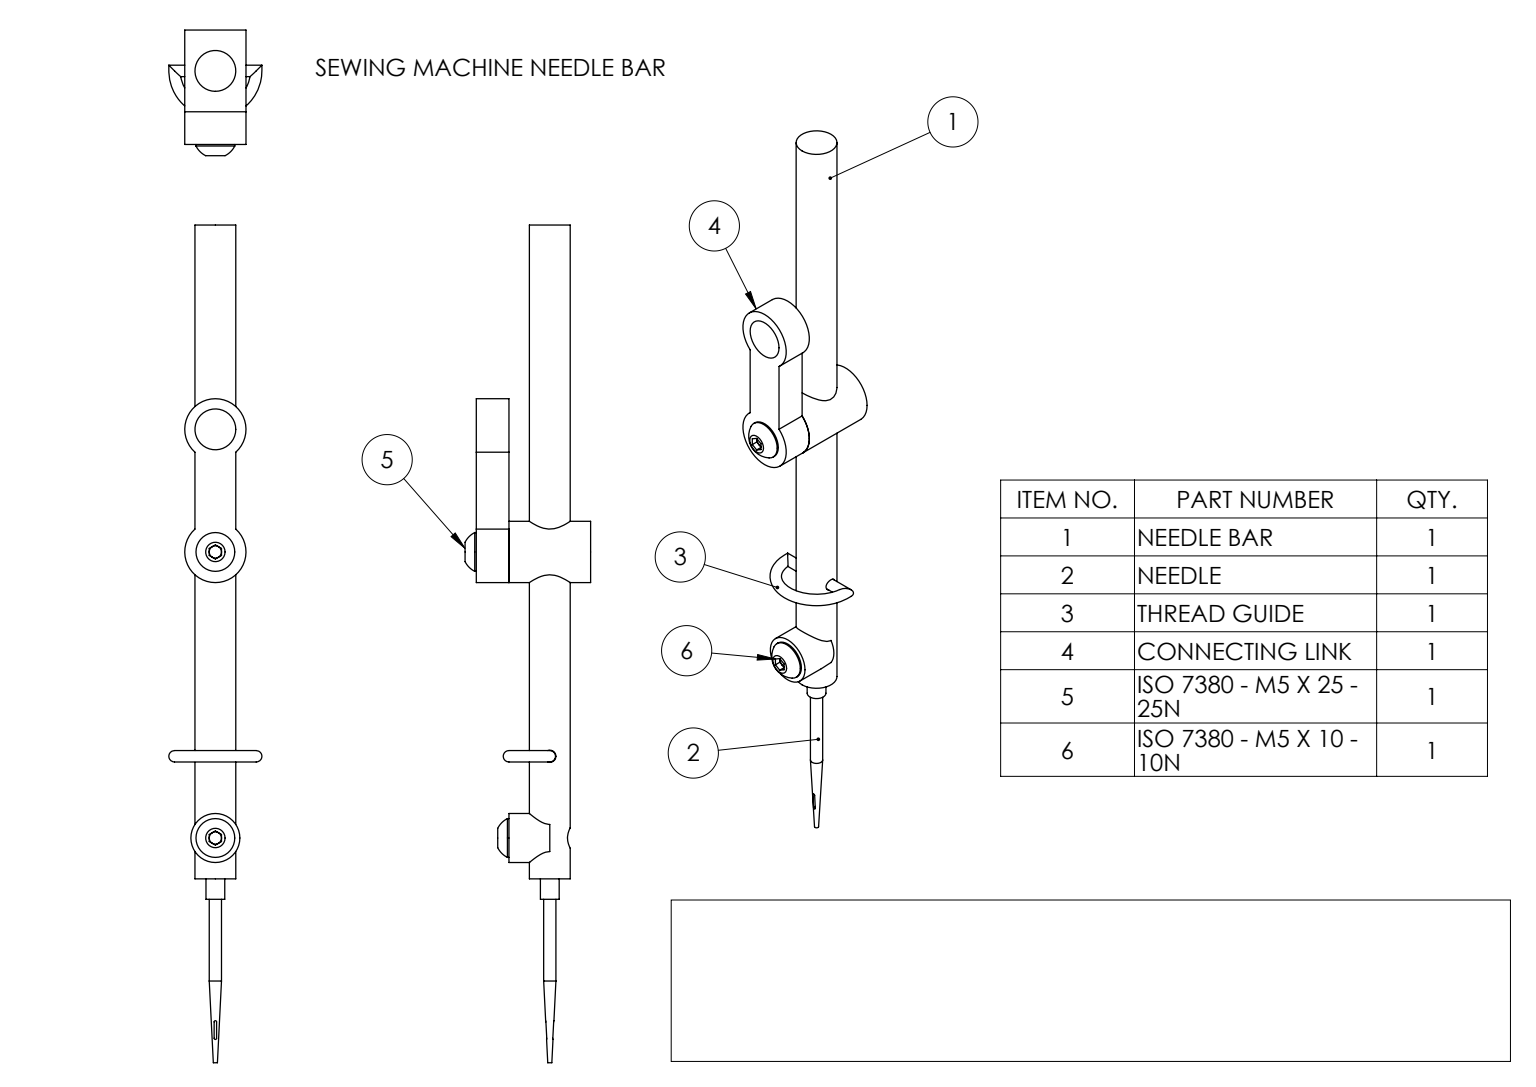
ISO-10303-21;
HEADER;
FILE_DESCRIPTION (('STEP AP214'),
    '1' );
FILE_NAME ('MAS-169',
    '2026-10-25T11:00:22',
    ( '' ),
    ( '' ),
    'SwSTEP 2.0',
    'SolidWorks 2026',
    '' );
FILE_SCHEMA (( 'AUTOMOTIVE_DESIGN' ));
ENDSEC;

DATA;
#1 = CARTESIAN_POINT ( 'NONE',  ( -6.877134118866000456, -50.00000000000000000, 5.285102517561346858 ) ) ;
#2 = CARTESIAN_POINT ( 'NONE',  ( 11.39999999999999680, -52.79999999999999716, -0.5466666666666269991 ) ) ;
#3 = ORIENTED_EDGE ( 'NONE', *, *, #2173, .T. ) ;
#4 = CARTESIAN_POINT ( 'NONE',  ( 4.999998311775604165, -51.49999437258534130, 0.09894250604207632804 ) ) ;
#5 = SHAPE_DEFINITION_REPRESENTATION ( #2134, #457 ) ;
#6 = CYLINDRICAL_SURFACE ( 'NONE', #1532, 4.999999999999999112 ) ;
#7 = CARTESIAN_POINT ( 'NONE',  ( -0.1736799743064503798, -76.00000000000005684, 5.000000000000000000 ) ) ;
#8 = UNCERTAINTY_MEASURE_WITH_UNIT (LENGTH_MEASURE( 1.000000000000000082E-05 ), #1107, 'distance_accuracy_value', 'NONE');
#9 =( BOUNDED_SURFACE ( )  B_SPLINE_SURFACE ( 3, 3, ( 
 ( #2907, #429, #2418, #2187, #1154, #2219, #2974, #1713, #2728, #2169, #3178, #2938, #2958, #2662, #1219, #461, #1468, #698, #2482, #1435, #1899, #2449, #446, #1450, #649, #2462, #2236, #1651, #919, #1916, #663, #189, #680, #1664, #2679, #1419, #2432, #1171 ),
 ( #1682, #1596, #593, #2589, #838, #2249, #321, #302, #69, #2812, #1788, #1838, #1822, #2342, #3004, #817, #221, #2743, #3255, #1078, #1549, #337, #2094, #1730, #1292, #477, #787, #726, #801, #2001, #1486, #2308, #35, #2797, #984, #1343, #1045, #2610 ),
 ( #1233, #3101, #969, #2498, #1313, #2829, #1806, #2077, #1985, #559, #540, #2056, #2554, #1328, #2847, #2358, #2989, #285, #3065, #1561, #2324, #2567, #52, #1064, #3081, #575, #1578, #884, #87, #2898, #388, #899, #2112, #1910, #2672, #2930, #2396, #671 ),
 ( #372, #1672, #2689, #855, #150, #2916, #657, #3139, #1613, #1892, #2377, #3120, #2426, #2628, #912, #1163, #1925, #1131, #122, #2145, #1855, #3152, #2131, #1097, #2866, #2181, #1412, #643, #872, #608, #3185, #1629, #1644, #1873, #420, #2411, #1428, #1658 ),
 ( #355, #3169, #107, #2882, #627, #1362, #1116, #402, #2642, #1381, #2658, #1395, #134, #1145, #2162, #438, #2194, #736, #994, #1194, #961, #487, #1496, #2504, #1179, #2257, #705, #3234, #2210, #2763, #1476, #228, #1993, #453, #2492, #1444, #214, #1227 ),
 ( #1241, #167, #2751, #2011, #3265, #2456, #720, #499, #182, #2736, #3213, #3199, #1741, #3013, #943, #1978, #752, #1753, #2441, #2243, #1691, #927, #1961, #1941, #2967, #2949, #688, #2707, #2722, #1705, #1458, #2474, #2228, #198, #1210, #2981, #1722, #470 ),
 ( #3249, #975, #2998, #813, #765, #315, #1507, #1256, #797, #1307, #2303, #2564, #2519, #31, #1, #1784, #1768, #1817, #2823, #571, #1574, #1011, #2026, #1544, #2808, #2271, #830, #1323, #2582, #1801, #2338, #1039, #246, #2052, #554, #2319, #3026, #48 ) ),
 .UNSPECIFIED., .T., .F., .F. ) 
 B_SPLINE_SURFACE_WITH_KNOTS ( ( 4, 3, 4 ),
 ( 4, 2, 2, 2, 2, 2, 2, 2, 2, 2, 2, 2, 2, 2, 2, 2, 2, 2, 4 ),
 ( 0.000000000000000000, 0.5000000000000000000, 1.000000000000000000 ),
 ( -0.05205660780589810299, -0.02602830390294905150, 0.000000000000000000, 0.01562500000000000000, 0.03125000000000000000, 0.06250000000000000000, 0.1250000000000000000, 0.2500000000000000000, 0.3750000000000000000, 0.5000000000000000000, 0.6250000000000000000, 0.7500000000000000000, 0.8750000000000000000, 0.9375000000000000000, 0.9687500000000000000, 0.9843750000000000000, 1.000000000000000000, 1.026028303902949190, 1.052056607805898381 ),
 .UNSPECIFIED. ) 
 GEOMETRIC_REPRESENTATION_ITEM ( )  RATIONAL_B_SPLINE_SURFACE ( (
 ( 1.000000000000000000, 1.000000000000000000, 1.000000000000000000, 1.000000000000000000, 1.000000000000000000, 1.000000000000000000, 1.000000000000000000, 1.000000000000000000, 1.000000000000000000, 1.000000000000000000, 1.000000000000000000, 1.000000000000000000, 1.000000000000000000, 1.000000000000000000, 1.000000000000000000, 1.000000000000000000, 1.000000000000000000, 1.000000000000000000, 1.000000000000000000, 1.000000000000000000, 1.000000000000000000, 1.000000000000000000, 1.000000000000000000, 1.000000000000000000, 1.000000000000000000, 1.000000000000000000, 1.000000000000000000, 1.000000000000000000, 1.000000000000000000, 1.000000000000000000, 1.000000000000000000, 1.000000000000000000, 1.000000000000000000, 1.000000000000000000, 1.000000000000000000, 1.000000000000000000, 1.000000000000000000, 1.000000000000000000),
 ( 0.3333333333333333703, 0.3333333333333333703, 0.3333333333333333703, 0.3333333333333333703, 0.3333333333333333703, 0.3333333333333333703, 0.3333333333333333703, 0.3333333333333333703, 0.3333333333333333703, 0.3333333333333333703, 0.3333333333333333703, 0.3333333333333333703, 0.3333333333333333703, 0.3333333333333333703, 0.3333333333333333703, 0.3333333333333333703, 0.3333333333333333703, 0.3333333333333333703, 0.3333333333333333703, 0.3333333333333333703, 0.3333333333333333703, 0.3333333333333333703, 0.3333333333333333703, 0.3333333333333333703, 0.3333333333333333703, 0.3333333333333333703, 0.3333333333333333703, 0.3333333333333333703, 0.3333333333333333703, 0.3333333333333333703, 0.3333333333333333703, 0.3333333333333333703, 0.3333333333333333703, 0.3333333333333333703, 0.3333333333333333703, 0.3333333333333333703, 0.3333333333333333703, 0.3333333333333333703),
 ( 0.3333333333333333703, 0.3333333333333333703, 0.3333333333333333703, 0.3333333333333333703, 0.3333333333333333703, 0.3333333333333333703, 0.3333333333333333703, 0.3333333333333333703, 0.3333333333333333703, 0.3333333333333333703, 0.3333333333333333703, 0.3333333333333333703, 0.3333333333333333703, 0.3333333333333333703, 0.3333333333333333703, 0.3333333333333333703, 0.3333333333333333703, 0.3333333333333333703, 0.3333333333333333703, 0.3333333333333333703, 0.3333333333333333703, 0.3333333333333333703, 0.3333333333333333703, 0.3333333333333333703, 0.3333333333333333703, 0.3333333333333333703, 0.3333333333333333703, 0.3333333333333333703, 0.3333333333333333703, 0.3333333333333333703, 0.3333333333333333703, 0.3333333333333333703, 0.3333333333333333703, 0.3333333333333333703, 0.3333333333333333703, 0.3333333333333333703, 0.3333333333333333703, 0.3333333333333333703),
 ( 1.000000000000000000, 1.000000000000000000, 1.000000000000000000, 1.000000000000000000, 1.000000000000000000, 1.000000000000000000, 1.000000000000000000, 1.000000000000000000, 1.000000000000000000, 1.000000000000000000, 1.000000000000000000, 1.000000000000000000, 1.000000000000000000, 1.000000000000000000, 1.000000000000000000, 1.000000000000000000, 1.000000000000000000, 1.000000000000000000, 1.000000000000000000, 1.000000000000000000, 1.000000000000000000, 1.000000000000000000, 1.000000000000000000, 1.000000000000000000, 1.000000000000000000, 1.000000000000000000, 1.000000000000000000, 1.000000000000000000, 1.000000000000000000, 1.000000000000000000, 1.000000000000000000, 1.000000000000000000, 1.000000000000000000, 1.000000000000000000, 1.000000000000000000, 1.000000000000000000, 1.000000000000000000, 1.000000000000000000),
 ( 0.3333333333333333703, 0.3333333333333333703, 0.3333333333333333703, 0.3333333333333333703, 0.3333333333333333703, 0.3333333333333333703, 0.3333333333333333703, 0.3333333333333333703, 0.3333333333333333703, 0.3333333333333333703, 0.3333333333333333703, 0.3333333333333333703, 0.3333333333333333703, 0.3333333333333333703, 0.3333333333333333703, 0.3333333333333333703, 0.3333333333333333703, 0.3333333333333333703, 0.3333333333333333703, 0.3333333333333333703, 0.3333333333333333703, 0.3333333333333333703, 0.3333333333333333703, 0.3333333333333333703, 0.3333333333333333703, 0.3333333333333333703, 0.3333333333333333703, 0.3333333333333333703, 0.3333333333333333703, 0.3333333333333333703, 0.3333333333333333703, 0.3333333333333333703, 0.3333333333333333703, 0.3333333333333333703, 0.3333333333333333703, 0.3333333333333333703, 0.3333333333333333703, 0.3333333333333333703),
 ( 0.3333333333333333703, 0.3333333333333333703, 0.3333333333333333703, 0.3333333333333333703, 0.3333333333333333703, 0.3333333333333333703, 0.3333333333333333703, 0.3333333333333333703, 0.3333333333333333703, 0.3333333333333333703, 0.3333333333333333703, 0.3333333333333333703, 0.3333333333333333703, 0.3333333333333333703, 0.3333333333333333703, 0.3333333333333333703, 0.3333333333333333703, 0.3333333333333333703, 0.3333333333333333703, 0.3333333333333333703, 0.3333333333333333703, 0.3333333333333333703, 0.3333333333333333703, 0.3333333333333333703, 0.3333333333333333703, 0.3333333333333333703, 0.3333333333333333703, 0.3333333333333333703, 0.3333333333333333703, 0.3333333333333333703, 0.3333333333333333703, 0.3333333333333333703, 0.3333333333333333703, 0.3333333333333333703, 0.3333333333333333703, 0.3333333333333333703, 0.3333333333333333703, 0.3333333333333333703),
 ( 1.000000000000000000, 1.000000000000000000, 1.000000000000000000, 1.000000000000000000, 1.000000000000000000, 1.000000000000000000, 1.000000000000000000, 1.000000000000000000, 1.000000000000000000, 1.000000000000000000, 1.000000000000000000, 1.000000000000000000, 1.000000000000000000, 1.000000000000000000, 1.000000000000000000, 1.000000000000000000, 1.000000000000000000, 1.000000000000000000, 1.000000000000000000, 1.000000000000000000, 1.000000000000000000, 1.000000000000000000, 1.000000000000000000, 1.000000000000000000, 1.000000000000000000, 1.000000000000000000, 1.000000000000000000, 1.000000000000000000, 1.000000000000000000, 1.000000000000000000, 1.000000000000000000, 1.000000000000000000, 1.000000000000000000, 1.000000000000000000, 1.000000000000000000, 1.000000000000000000, 1.000000000000000000, 1.000000000000000000) ) ) 
 REPRESENTATION_ITEM ( '' )  SURFACE ( )  );
#10 = DIRECTION ( 'NONE',  ( -1.000000000000000000, 0.000000000000000000, 0.000000000000000000 ) ) ;
#11 = CARTESIAN_POINT ( 'NONE',  ( 0.000000000000000000, -125.0000000000000000, 0.4999999999999813483 ) ) ;
#12 = CARTESIAN_POINT ( 'NONE',  ( 8.609154349733209699, -50.54332563323345795, 1.294262817214646644 ) ) ;
#13 = CARTESIAN_POINT ( 'NONE',  ( -8.530791689320901483, -50.00000000000000000, 1.124695299888049504 ) ) ;
#14 = VERTEX_POINT ( 'NONE', #1452 ) ;
#15 = EDGE_CURVE ( 'NONE', #50, #1696, #42, .T. ) ;
#16 = CARTESIAN_POINT ( 'NONE',  ( 0.2999999999999837796, -118.9999999999982379, -0.7416198487096254954 ) ) ;
#17 = CARTESIAN_POINT ( 'NONE',  ( 0.3311419820765648669, -72.48349571540411773, -4.991687326893459620 ) ) ;
#18 = CARTESIAN_POINT ( 'NONE',  ( 2.499999999999999556, 3.061616997868382648E-16, 10.00000000000000000 ) ) ;
#19 = CARTESIAN_POINT ( 'NONE',  ( -5.000000000000000000, 5.590169943749474513, 10.00000000000000000 ) ) ;
#20 = ORIENTED_EDGE ( 'NONE', *, *, #1771, .F. ) ;
#21 = CARTESIAN_POINT ( 'NONE',  ( 4.769696007084727185, -50.19647014491117432, 1.499999999999993339 ) ) ;
#22 = ADVANCED_FACE ( 'NONE', ( #937 ), #2745, .F. ) ;
#23 = SHAPE_DEFINITION_REPRESENTATION ( #2632, #3271 ) ;
#24 = CARTESIAN_POINT ( 'NONE',  ( -4.828212536628694984, -50.75366254478191053, 1.300578314244078992 ) ) ;
#25 = CYLINDRICAL_SURFACE ( 'NONE', #3173, 4.999999999999999112 ) ;
#26 = CARTESIAN_POINT ( 'NONE',  ( 3.061616997868384127E-16, -72.50000000000001421, 2.500000000000000444 ) ) ;
#27 = DIRECTION ( 'NONE',  ( -0.000000000000000000, -0.000000000000000000, -1.000000000000000000 ) ) ;
#28 = CARTESIAN_POINT ( 'NONE',  ( 7.513445500750180805, -50.00000000000000000, 4.333070140107198043 ) ) ;
#29 = EDGE_LOOP ( 'NONE', ( #3142, #458 ) ) ;
#30 =( LENGTH_UNIT ( ) NAMED_UNIT ( * ) SI_UNIT ( .MILLI., .METRE. ) );
#31 = CARTESIAN_POINT ( 'NONE',  ( -7.513445500749800665, -50.00000000000000000, 4.333070140105378165 ) ) ;
#32 = DIRECTION ( 'NONE',  ( -0.000000000000000000, -0.000000000000000000, -1.000000000000000000 ) ) ;
#33 = ORIENTED_EDGE ( 'NONE', *, *, #1677, .F. ) ;
#34 = CARTESIAN_POINT ( 'NONE',  ( 4.871330634494102974, -50.99215130299450038, -1.129198576418441791 ) ) ;
#35 = CARTESIAN_POINT ( 'NONE',  ( 8.599996472200352571, -47.20000000000001705, 0.1525981975067867147 ) ) ;
#36 = EDGE_CURVE ( 'NONE', #2171, #1853, #1673, .T. ) ;
#37 = CIRCLE ( 'NONE', #1306, 7.500000000000000000 ) ;
#38 = VERTEX_POINT ( 'NONE', #728 ) ;
#39 = CARTESIAN_POINT ( 'NONE',  ( -3.982914377913044479, -74.49364316089672400, 3.038300766938668573 ) ) ;
#40 = PRODUCT_DEFINITION_CONTEXT ( 'detailed design', #391, 'design' ) ;
#41 = CARTESIAN_POINT ( 'NONE',  ( -7.500000000000000000, -50.00000000000000000, -1.500000000000006439 ) ) ;
#42 = B_SPLINE_CURVE_WITH_KNOTS ( 'NONE', 3,
 ( #682, #3227, #1437, #2189, #1490, #1684, #3257, #223, #987, #191, #2464, #1205, #3193, #956 ),
 .UNSPECIFIED., .F., .F.,
 ( 4, 2, 2, 2, 2, 2, 4 ),
 ( -7.483321455827298351E-06, 0.0006606241027954298925, 0.001328731527046687205, 0.001662785239172322529, 0.001996838951297958287, 0.002330892663423593178, 0.002664946375549228936 ),
 .UNSPECIFIED. ) ;
#43 = DIRECTION ( 'NONE',  ( 1.000000000000000000, -0.000000000000000000, -0.000000000000000000 ) ) ;
#44 = CARTESIAN_POINT ( 'NONE',  ( 8.599996472200352571, -50.00000000000000000, 0.1525981975067866592 ) ) ;
#45 = ORIENTED_EDGE ( 'NONE', *, *, #3043, .T. ) ;
#46 = DIRECTION ( 'NONE',  ( 0.000000000000000000, 1.000000000000000000, 0.000000000000000000 ) ) ;
#47 = AXIS2_PLACEMENT_3D ( 'NONE', #892, #615, #1900 ) ;
#48 = CARTESIAN_POINT ( 'NONE',  ( 8.599999999999996092, -50.00000000000000000, -1.639999999999997460 ) ) ;
#49 = CARTESIAN_POINT ( 'NONE',  ( -6.610444160707455418E-15, -72.50000000000009948, -5.000000000000047962 ) ) ;
#50 = VERTEX_POINT ( 'NONE', #715 ) ;
#51 = CARTESIAN_POINT ( 'NONE',  ( 4.977204064302565456, -51.42262508310333402, -0.4855051584829146449 ) ) ;
#52 = CARTESIAN_POINT ( 'NONE',  ( 7.005833569766282132, -47.20000000000001705, 9.116201041261453142 ) ) ;
#53 = CIRCLE ( 'NONE', #2065, 4.999999999999999112 ) ;
#54 = ADVANCED_FACE ( 'NONE', ( #463, #744 ), #700, .T. ) ;
#55 = CARTESIAN_POINT ( 'NONE',  ( -0.3471650268615569246, -75.99247303379605967, 4.990975288187767589 ) ) ;
#56 = ADVANCED_FACE ( 'NONE', ( #1470 ), #1700, .T. ) ;
#57 = CARTESIAN_POINT ( 'NONE',  ( 0.000000000000000000, 0.000000000000000000, 10.00000000000000000 ) ) ;
#58 = ORIENTED_EDGE ( 'NONE', *, *, #3093, .T. ) ;
#59 = EDGE_CURVE ( 'NONE', #1569, #129, #2568, .T. ) ;
#60 = CARTESIAN_POINT ( 'NONE',  ( 4.999999999999999112, 30.00000000000000000, 18.00000000000000355 ) ) ;
#61 = CARTESIAN_POINT ( 'NONE',  ( 1.125736483476999839, -50.00000000000000000, 8.599999999999996092 ) ) ;
#62 = ORIENTED_EDGE ( 'NONE', *, *, #59, .F. ) ;
#63 = CARTESIAN_POINT ( 'NONE',  ( 8.572527594031472993E-15, -70.00000000000000000, 10.00000000000000000 ) ) ;
#64 = CARTESIAN_POINT ( 'NONE',  ( -2.499999999999995559, -70.00000000000000000, 0.000000000000000000 ) ) ;
#65 = CARTESIAN_POINT ( 'NONE',  ( 4.964478897467096807, -5.622442520179988357, 0.6821754209311353678 ) ) ;
#66 = CARTESIAN_POINT ( 'NONE',  ( -9.999999999999998224, -48.60000000000000142, 1.734719587726169024E-19 ) ) ;
#67 = VERTEX_POINT ( 'NONE', #238 ) ;
#68 = CARTESIAN_POINT ( 'NONE',  ( -0.6778607859896496057, 7.476644527972223564, 4.965157125901431101 ) ) ;
#69 = CARTESIAN_POINT ( 'NONE',  ( -8.572276570256935457, -47.20000000000001705, 0.7042094815226510596 ) ) ;
#70 = ORIENTED_EDGE ( 'NONE', *, *, #2414, .T. ) ;
#71 = CARTESIAN_POINT ( 'NONE',  ( -7.500000000000000000, 0.000000000000000000, 10.00000000000000000 ) ) ;
#72 = ADVANCED_FACE ( 'NONE', ( #1264 ), #1017, .F. ) ;
#73 = CARTESIAN_POINT ( 'NONE',  ( 5.000000000000000000, 24.40983005625052726, 18.00000000000000355 ) ) ;
#74 = VERTEX_POINT ( 'NONE', #2785 ) ;
#75 =( LENGTH_UNIT ( ) NAMED_UNIT ( * ) SI_UNIT ( .MILLI., .METRE. ) );
#76 = DIRECTION ( 'NONE',  ( -0.000000000000000000, -0.000000000000000000, 1.000000000000000000 ) ) ;
#77 = CARTESIAN_POINT ( 'NONE',  ( -4.331939449206426929, -50.00000000000000000, 7.514224851276241957 ) ) ;
#78 = ORIENTED_EDGE ( 'NONE', *, *, #1919, .T. ) ;
#79 = CARTESIAN_POINT ( 'NONE',  ( 8.572527594031472993E-15, -70.00000000000000000, 10.00000000000000000 ) ) ;
#80 =( LENGTH_UNIT ( ) NAMED_UNIT ( * ) SI_UNIT ( .MILLI., .METRE. ) );
#81 = CARTESIAN_POINT ( 'NONE',  ( 4.966432541228214426, 5.620714496023337503, -0.6691698110145376521 ) ) ;
#82 = CARTESIAN_POINT ( 'NONE',  ( 4.821318589555972700, -5.745344196342314191, 1.334996645354991074 ) ) ;
#83 = CARTESIAN_POINT ( 'NONE',  ( 7.513445500750180805, -50.00000000000000000, 4.333070140107198043 ) ) ;
#84 = VERTEX_POINT ( 'NONE', #2265 ) ;
#85 = CYLINDRICAL_SURFACE ( 'NONE', #3102, 2.499999999999999556 ) ;
#86 = AXIS2_PLACEMENT_3D ( 'NONE', #2225, #1782, #1240 ) ;
#87 = CARTESIAN_POINT ( 'NONE',  ( 11.30825875096014066, -47.20000000000001705, 1.490875164968454625 ) ) ;
#88 = ORIENTED_EDGE ( 'NONE', *, *, #36, .T. ) ;
#89 = CARTESIAN_POINT ( 'NONE',  ( -2.483686021788606091, -70.33016769071190311, -4.339668646282463627 ) ) ;
#90 = CIRCLE ( 'NONE', #990, 6.000000000000001776 ) ;
#91 = CARTESIAN_POINT ( 'NONE',  ( -2.250215587473127332, -50.00000000000000000, 8.376503107917878665 ) ) ;
#92 = ORIENTED_EDGE ( 'NONE', *, *, #2004, .F. ) ;
#93 = VECTOR ( 'NONE', #127, 1000.000000000000000 ) ;
#94 = CARTESIAN_POINT ( 'NONE',  ( -0.8154661022227107647, -67.63113994865679501, -4.935425033279029705 ) ) ;
#95 = DIRECTION ( 'NONE',  ( -0.000000000000000000, 0.000000000000000000, 1.000000000000000000 ) ) ;
#96 = FACE_OUTER_BOUND ( 'NONE', #2631, .T. ) ;
#97 = VERTEX_POINT ( 'NONE', #26 ) ;
#98 = EDGE_CURVE ( 'NONE', #842, #2258, #2815, .T. ) ;
#99 = CARTESIAN_POINT ( 'NONE',  ( 0.2999999999999837796, -118.9999999999982379, 0.7416198487096254954 ) ) ;
#100 = CARTESIAN_POINT ( 'NONE',  ( 2.543133226181223616, 7.061565991568797607, 4.317068135836759524 ) ) ;
#101 = CARTESIAN_POINT ( 'NONE',  ( -0.3480864936855371794, -64.00754952754900273, 4.990948402655851268 ) ) ;
#102 = VERTEX_POINT ( 'NONE', #3084 ) ;
#103 = CARTESIAN_POINT ( 'NONE',  ( -4.327080376399232264, 6.129587957101251483, -2.525419289280399049 ) ) ;
#104 = EDGE_CURVE ( 'NONE', #67, #74, #1503, .T. ) ;
#105 = ADVANCED_FACE ( 'NONE', ( #527 ), #307, .F. ) ;
#106 = AXIS2_PLACEMENT_3D ( 'NONE', #3179, #664, #3192 ) ;
#107 = CARTESIAN_POINT ( 'NONE',  ( -11.39999999999999680, -52.79999999999999716, -1.093333333333363022 ) ) ;
#108 = PRESENTATION_LAYER_ASSIGNMENT (  '', '', ( #480 ) ) ;
#109 = FACE_OUTER_BOUND ( 'NONE', #857, .T. ) ;
#110 = CARTESIAN_POINT ( 'NONE',  ( 0.2999999999999999889, -114.9999999999982236, 0.9539392014169838507 ) ) ;
#111 = ORIENTED_EDGE ( 'NONE', *, *, #929, .T. ) ;
#112 = DIRECTION ( 'NONE',  ( 1.000000000000000000, 0.000000000000000000, 0.000000000000000000 ) ) ;
#113 = DIRECTION ( 'NONE',  ( 1.000000000000000000, 0.000000000000000000, 0.000000000000000000 ) ) ;
#114 = CARTESIAN_POINT ( 'NONE',  ( 8.599999999999996092, -50.00000000000000000, -0.5466666666666269991 ) ) ;
#115 = EDGE_LOOP ( 'NONE', ( #2950, #3054 ) ) ;
#116 = CARTESIAN_POINT ( 'NONE',  ( 8.572527594031472993E-15, -70.00000000000000000, 10.00000000000000000 ) ) ;
#117 = SHAPE_REPRESENTATION_RELATIONSHIP ( 'NONE' , 'NONE' ,  #2799, #1401 ) ;
#118 = CARTESIAN_POINT ( 'NONE',  ( 4.728889495302424528, 5.823500886956166411, 1.655898480698586139 ) ) ;
#119 = CARTESIAN_POINT ( 'NONE',  ( -1.492255338562904265, -47.20000000000001705, 11.39999999999999680 ) ) ;
#120 = PRODUCT_DEFINITION_SHAPE ( 'NONE', 'NONE',  #3277 ) ;
#121 = DIRECTION ( 'NONE',  ( 0.000000000000000000, -1.000000000000000000, 0.000000000000000000 ) ) ;
#122 = CARTESIAN_POINT ( 'NONE',  ( -1.492255338562904043, -50.00000000000000000, 11.39999999999999680 ) ) ;
#123 = VERTEX_POINT ( 'NONE', #544 ) ;
#124 = CARTESIAN_POINT ( 'NONE',  ( 0.000000000000000000, -125.0000000000000000, 0.000000000000000000 ) ) ;
#125 = ORIENTED_EDGE ( 'NONE', *, *, #751, .F. ) ;
#126 = CARTESIAN_POINT ( 'NONE',  ( 0.2671776428991994301, -119.1571283586499845, 0.7478606154414358942 ) ) ;
#127 = DIRECTION ( 'NONE',  ( -1.000000000000000000, -0.000000000000000000, -0.000000000000000000 ) ) ;
#128 = CARTESIAN_POINT ( 'NONE',  ( 0.8153798621788117540, -67.63100920925315052, -4.935481307755256175 ) ) ;
#129 = VERTEX_POINT ( 'NONE', #509 ) ;
#130 = CARTESIAN_POINT ( 'NONE',  ( 0.000000000000000000, -80.00000000000000000, 4.999999999999999112 ) ) ;
#131 = CARTESIAN_POINT ( 'NONE',  ( 11.39999999999999680, -47.20000000000001705, -0.5466666666666269991 ) ) ;
#132 =( LENGTH_UNIT ( ) NAMED_UNIT ( * ) SI_UNIT ( .MILLI., .METRE. ) );
#133 = CARTESIAN_POINT ( 'NONE',  ( -4.964478897467096807, 5.622442520179988357, 0.6821754209311353678 ) ) ;
#134 = CARTESIAN_POINT ( 'NONE',  ( -10.81682914263834405, -52.79999999999999716, 3.675996170188739143 ) ) ;
#135 = EDGE_LOOP ( 'NONE', ( #2013, #111, #33, #444, #818, #2129 ) ) ;
#136 = EDGE_CURVE ( 'NONE', #870, #2195, #2997, .T. ) ;
#137 = CARTESIAN_POINT ( 'NONE',  ( -8.767617449782825645, -49.18583174968846805, 1.157007882117286446 ) ) ;
#138 = AXIS2_PLACEMENT_3D ( 'NONE', #166, #181, #437 ) ;
#139 = ORIENTED_EDGE ( 'NONE', *, *, #3025, .T. ) ;
#140 = CARTESIAN_POINT ( 'NONE',  ( 0.1569248533674419965, -119.2672972209964399, 0.7728889768974943619 ) ) ;
#141 = CLOSED_SHELL ( 'NONE', ( #340, #1948, #3100, #1050 ) ) ;
#142 = CARTESIAN_POINT ( 'NONE',  ( 0.000000000000000000, 0.000000000000000000, 10.00000000000000000 ) ) ;
#143 = DIRECTION ( 'NONE',  ( 0.000000000000000000, -0.000000000000000000, 1.000000000000000000 ) ) ;
#144 = ORIENTED_EDGE ( 'NONE', *, *, #2783, .T. ) ;
#145 = CIRCLE ( 'NONE', #415, 4.999999999999999112 ) ;
#146 = DIRECTION ( 'NONE',  ( -0.000000000000000000, -0.000000000000000000, -1.000000000000000000 ) ) ;
#147 = CARTESIAN_POINT ( 'NONE',  ( 11.03470001049147697, -47.20000000000001705, 2.958453039086267111 ) ) ;
#148 = CARTESIAN_POINT ( 'NONE',  ( -3.971589419094359030, -6.365665093354385462, -3.054047635831909524 ) ) ;
#149 = CARTESIAN_POINT ( 'NONE',  ( -10.97094949647943274, -51.01251636945237777, -0.9709494964794268546 ) ) ;
#150 = CARTESIAN_POINT ( 'NONE',  ( -11.40000778997679021, -50.00000000000000000, -0.2924664341913127408 ) ) ;
#151 = ORIENTED_EDGE ( 'NONE', *, *, #320, .T. ) ;
#152 = AXIS2_PLACEMENT_3D ( 'NONE', #2297, #2784, #10 ) ;
#153 = CYLINDRICAL_SURFACE ( 'NONE', #3180, 2.499999999999999556 ) ;
#154 = VECTOR ( 'NONE', #1851, 1000.000000000000000 ) ;
#155 = CARTESIAN_POINT ( 'NONE',  ( 0.000000000000000000, 0.000000000000000000, -10.00000000000000000 ) ) ;
#156 = EDGE_CURVE ( 'NONE', #3170, #1754, #1004, .T. ) ;
#157 = ORIENTED_EDGE ( 'NONE', *, *, #592, .T. ) ;
#158 = CARTESIAN_POINT ( 'NONE',  ( 7.500000000000000000, 9.184850993605147944E-16, 10.00000000000000000 ) ) ;
#159 = CARTESIAN_POINT ( 'NONE',  ( 9.354236102686614984, -48.73731279115568071, 0.6262106814100325547 ) ) ;
#160 = CARTESIAN_POINT ( 'NONE',  ( 4.823113930341509814, -73.57101484999542151, 1.361197559098670462 ) ) ;
#161 = EDGE_CURVE ( 'NONE', #1969, #1853, #1067, .T. ) ;
#162 = CARTESIAN_POINT ( 'NONE',  ( -4.997074555615626856, -48.50966683676461599, -0.1965204501117691904 ) ) ;
#163 = CARTESIAN_POINT ( 'NONE',  ( -10.81682914263834405, -50.00000000000000000, 3.675996170188739143 ) ) ;
#164 = CARTESIAN_POINT ( 'NONE',  ( -11.39999532361432522, -50.00000000000000000, 0.1755699507458657049 ) ) ;
#165 = ADVANCED_FACE ( 'NONE', ( #1515, #3069 ), #289, .T. ) ;
#166 = CARTESIAN_POINT ( 'NONE',  ( 0.000000000000000000, 30.00000000000000000, 18.00000000000000355 ) ) ;
#167 = CARTESIAN_POINT ( 'NONE',  ( -8.599999999999996092, -52.79999999999999716, -1.366666666666159546 ) ) ;
#168 = ORIENTED_EDGE ( 'NONE', *, *, #196, .T. ) ;
#169 = CARTESIAN_POINT ( 'NONE',  ( -8.582665138674013150, -50.00000000000000000, 0.5636706063486749407 ) ) ;
#170 = CARTESIAN_POINT ( 'NONE',  ( -4.999999999999999112, -73.31662479035540514, 0.000000000000000000 ) ) ;
#171 = CARTESIAN_POINT ( 'NONE',  ( -5.999999999999992895, -70.00000000000000000, 0.000000000000000000 ) ) ;
#172 = ORIENTED_EDGE ( 'NONE', *, *, #2667, .F. ) ;
#173 = CARTESIAN_POINT ( 'NONE',  ( 0.1736799743064505464, -64.00000000000000000, 5.000000000000000000 ) ) ;
#174 = B_SPLINE_CURVE_WITH_KNOTS ( 'NONE', 3,
 ( #727, #1234, #2700, #1436, #190, #493, #2002, #3005, #1747, #2526, #526, #1263 ),
 .UNSPECIFIED., .F., .F.,
 ( 4, 2, 2, 2, 2, 4 ),
 ( 0.002664946375549201180, 0.002999773306175300240, 0.003334600236801398866, 0.004004254098053579639, 0.004673907959305761278, 0.005343561820557941183 ),
 .UNSPECIFIED. ) ;
#175 = DIRECTION ( 'NONE',  ( 0.000000000000000000, -0.000000000000000000, -1.000000000000000000 ) ) ;
#176 = DIRECTION ( 'NONE',  ( 0.000000000000000000, 0.000000000000000000, -1.000000000000000000 ) ) ;
#177 = CARTESIAN_POINT ( 'NONE',  ( 0.6967678811844650877, -75.96197462185259042, 4.954315763534759220 ) ) ;
#178 = CARTESIAN_POINT ( 'NONE',  ( -4.769696007084725409, -50.00000000000000000, -1.500000000000006439 ) ) ;
#179 = CARTESIAN_POINT ( 'NONE',  ( -11.39539595717859299, -47.20000000000001705, 0.3739757293043587949 ) ) ;
#180 = CARTESIAN_POINT ( 'NONE',  ( 4.784663389310397363, -49.60983055069853265, -1.451689076663209566 ) ) ;
#181 = DIRECTION ( 'NONE',  ( -0.000000000000000000, -0.000000000000000000, -1.000000000000000000 ) ) ;
#182 = CARTESIAN_POINT ( 'NONE',  ( -8.572276570256935457, -52.79999999999999716, 0.7042094815226510596 ) ) ;
#183 = EDGE_LOOP ( 'NONE', ( #2116, #763, #2764, #874, #2899, #62, #1341 ) ) ;
#184 = CARTESIAN_POINT ( 'NONE',  ( -1.125736483476999839, -50.00000000000000000, 8.599999999999996092 ) ) ;
#185 = CARTESIAN_POINT ( 'NONE',  ( 1.259284006377631604, -72.16577835674955566, -4.840859579833913351 ) ) ;
#186 = CARTESIAN_POINT ( 'NONE',  ( 11.38641147205292725, -49.77694418854823510, -1.386411472052930804 ) ) ;
#187 = ORIENTED_EDGE ( 'NONE', *, *, #2783, .F. ) ;
#188 = CARTESIAN_POINT ( 'NONE',  ( 1.181079518071022826E-19, -64.00000000000000000, 4.999999999999999112 ) ) ;
#189 = CARTESIAN_POINT ( 'NONE',  ( 8.596526774713712626, -50.00000000000000000, 0.2821220414049827596 ) ) ;
#190 = CARTESIAN_POINT ( 'NONE',  ( -11.29810924534245586, -49.46572717680115971, -1.298109245342457418 ) ) ;
#191 = CARTESIAN_POINT ( 'NONE',  ( 11.29771452881883498, -50.53508261979053628, -1.297714528818850299 ) ) ;
#192 = CARTESIAN_POINT ( 'NONE',  ( -4.977204064302565456, -48.57737491689668730, -0.4855051584829146449 ) ) ;
#193 = VECTOR ( 'NONE', #1958, 1000.000000000000000 ) ;
#194 = CARTESIAN_POINT ( 'NONE',  ( -11.40000778997679198, -52.79999999999999716, -0.2924664341913127408 ) ) ;
#195 = CARTESIAN_POINT ( 'NONE',  ( 4.769696007084728073, -49.90173799037950886, 1.499999999999994449 ) ) ;
#196 = EDGE_CURVE ( 'NONE', #229, #14, #275, .T. ) ;
#197 = FACE_OUTER_BOUND ( 'NONE', #689, .T. ) ;
#198 = CARTESIAN_POINT ( 'NONE',  ( 8.600005876649037262, -52.79999999999999716, -0.2541998246239300374 ) ) ;
#199 = ORIENTED_EDGE ( 'NONE', *, *, #2749, .T. ) ;
#200 = CARTESIAN_POINT ( 'NONE',  ( -8.572276570256935457, -50.00000000000000000, 0.7042094815226510596 ) ) ;
#201 = CARTESIAN_POINT ( 'NONE',  ( 6.000000000000010658, -70.00000000000000000, 0.000000000000000000 ) ) ;
#202 = CARTESIAN_POINT ( 'NONE',  ( 9.999999999999976907, -48.60000000000000142, -1.084199742356775455E-20 ) ) ;
#203 = ORIENTED_EDGE ( 'NONE', *, *, #2410, .F. ) ;
#204 = CARTESIAN_POINT ( 'NONE',  ( 2.816687638038912549E-16, -84.99999999999998579, -2.300000000000000266 ) ) ;
#205 = AXIS2_PLACEMENT_3D ( 'NONE', #2839, #2602, #2103 ) ;
#206 = CARTESIAN_POINT ( 'NONE',  ( 0.000000000000000000, -84.99999999999998579, 0.000000000000000000 ) ) ;
#207 = DIRECTION ( 'NONE',  ( 1.000000000000000000, 0.000000000000000000, 0.000000000000000000 ) ) ;
#208 = CARTESIAN_POINT ( 'NONE',  ( 4.999999999999999112, -73.31662479035541935, 0.000000000000000000 ) ) ;
#209 = DIRECTION ( 'NONE',  ( 0.000000000000000000, -1.000000000000000000, 0.000000000000000000 ) ) ;
#210 = CARTESIAN_POINT ( 'NONE',  ( -9.959683570761574956, -52.79999999999999716, 5.743837162464267898 ) ) ;
#211 = CARTESIAN_POINT ( 'NONE',  ( 4.793458659903279795, -49.51492518266869780, 1.422772306546142174 ) ) ;
#212 = CARTESIAN_POINT ( 'NONE',  ( -11.39999999999999680, -50.11112248448768014, -1.400000000000000355 ) ) ;
#213 = ADVANCED_FACE ( 'NONE', ( #2558, #772 ), #1795, .T. ) ;
#214 = CARTESIAN_POINT ( 'NONE',  ( 11.39999999999999680, -52.79999999999999716, -1.366666666666861873 ) ) ;
#215 = APPLICATION_CONTEXT ( 'automotive_design' ) ;
#216 = VERTEX_POINT ( 'NONE', #1535 ) ;
#217 = CARTESIAN_POINT ( 'NONE',  ( 6.877134118866902845, -50.00000000000000000, 5.285102517562147995 ) ) ;
#218 = CARTESIAN_POINT ( 'NONE',  ( 3.078327448814686562, -6.845130131842670274, -3.953084837412474517 ) ) ;
#219 =( BOUNDED_CURVE ( )  B_SPLINE_CURVE ( 3, ( #377, #1897, #2151, #343 ),
 .UNSPECIFIED., .F., .F. ) 
 B_SPLINE_CURVE_WITH_KNOTS ( ( 4, 4 ),
 ( 3.141592653589794448, 4.712388980384689674 ),
 .UNSPECIFIED. ) 
 CURVE ( )  GEOMETRIC_REPRESENTATION_ITEM ( )  RATIONAL_B_SPLINE_CURVE ( ( 1.000000000000000000, 0.8047378541243652705, 0.8047378541243652705, 1.000000000000000000 ) ) 
 REPRESENTATION_ITEM ( '' )  );
#220 = FACE_OUTER_BOUND ( 'NONE', #2600, .T. ) ;
#221 = CARTESIAN_POINT ( 'NONE',  ( -4.331939449206426929, -47.20000000000001705, 7.514224851276242845 ) ) ;
#222 = DIRECTION ( 'NONE',  ( -0.000000000000000000, -0.000000000000000000, -1.000000000000000000 ) ) ;
#223 = CARTESIAN_POINT ( 'NONE',  ( 11.15228598338264732, -50.80068377669682889, -1.152285983382657086 ) ) ;
#224 = FACE_OUTER_BOUND ( 'NONE', #3125, .T. ) ;
#225 = CARTESIAN_POINT ( 'NONE',  ( 11.39999999999999680, -50.00000000000000000, -1.093333333333372126 ) ) ;
#226 = CARTESIAN_POINT ( 'NONE',  ( 4.769696007084729850, -50.00000000000000000, 1.499999999999994449 ) ) ;
#227 = SURFACE_SIDE_STYLE ('',( #2532 ) ) ;
#228 = CARTESIAN_POINT ( 'NONE',  ( 11.39539595717845799, -52.79999999999999716, 0.3739757293042010877 ) ) ;
#229 = VERTEX_POINT ( 'NONE', #1298 ) ;
#230 = EDGE_CURVE ( 'NONE', #2611, #2101, #2545, .T. ) ;
#231 = CARTESIAN_POINT ( 'NONE',  ( -8.582665138674013150, -47.20000000000001705, 0.5636706063486748297 ) ) ;
#232 = B_SPLINE_CURVE_WITH_KNOTS ( 'NONE', 3,
 ( #734, #2454, #2734, #180, #2224, #1192, #3011, #1751, #2761, #497, #2206, #3211, #468, #2748, #2964, #2268, #1506, #2517, #2503, #242, #1473, #3275, #2469, #211, #1938, #2720, #195, #226 ),
 .UNSPECIFIED., .F., .F.,
 ( 4, 2, 2, 2, 2, 2, 2, 2, 2, 2, 2, 2, 2, 4 ),
 ( 0.000000000000000000, 0.0002948077093299257545, 0.0005896154186598515090, 0.0008844231279897772635, 0.001179230837319703018, 0.001768846255979540866, 0.002358461674639378714, 0.002653269383969297963, 0.002948077093299216345, 0.003537692511959054844, 0.003832500221288973660, 0.004127307930618892041, 0.004422115639948811724, 0.004716923349278730540 ),
 .UNSPECIFIED. ) ;
#233 = CARTESIAN_POINT ( 'NONE',  ( -4.476097271599867256, -65.99976937466333027, 2.250477508087396661 ) ) ;
#234 = EDGE_CURVE ( 'NONE', #1786, #1583, #2021, .T. ) ;
#235 = DIRECTION ( 'NONE',  ( -0.000000000000000000, 1.000000000000000000, -0.000000000000000000 ) ) ;
#236 = UNCERTAINTY_MEASURE_WITH_UNIT (LENGTH_MEASURE( 1.000000000000000082E-05 ), #1255, 'distance_accuracy_value', 'NONE');
#237 = DIRECTION ( 'NONE',  ( 0.000000000000000000, 0.000000000000000000, 1.000000000000000000 ) ) ;
#238 = CARTESIAN_POINT ( 'NONE',  ( -2.300000000000000266, -72.60000000000000853, -1.734723475976807094E-15 ) ) ;
#239 = CIRCLE ( 'NONE', #570, 2.500000000000000000 ) ;
#240 = CARTESIAN_POINT ( 'NONE',  ( 8.572527594031472993E-15, -70.00000000000000000, 0.000000000000000000 ) ) ;
#241 = CARTESIAN_POINT ( 'NONE',  ( -1.492255338562904265, -52.79999999999999716, 11.39999999999999680 ) ) ;
#242 = CARTESIAN_POINT ( 'NONE',  ( 4.871060595381011993, -49.00914020874981247, 1.130390421582378124 ) ) ;
#243 = CIRCLE ( 'NONE', #1828, 7.500000000000000888 ) ;
#244 = FILL_AREA_STYLE ('',( #796 ) ) ;
#245 = VECTOR ( 'NONE', #2046, 1000.000000000000000 ) ;
#246 = CARTESIAN_POINT ( 'NONE',  ( 8.599996472200352571, -50.00000000000000000, 0.1525981975067866592 ) ) ;
#247 = ORIENTED_EDGE ( 'NONE', *, *, #1457, .T. ) ;
#248 = AXIS2_PLACEMENT_3D ( 'NONE', #2084, #843, #1137 ) ;
#249 = CARTESIAN_POINT ( 'NONE',  ( 4.793596727855903517, -50.48644371210733084, -1.422310562379361487 ) ) ;
#250 = APPLICATION_PROTOCOL_DEFINITION ( 'draft international standard', 'automotive_design', 1998, #215 ) ;
#251 = CARTESIAN_POINT ( 'NONE',  ( 4.666223265025314149, -5.872199985543652190, 1.803446265377422364 ) ) ;
#252 = CARTESIAN_POINT ( 'NONE',  ( 0.000000000000000000, 0.000000000000000000, 18.00000000000000355 ) ) ;
#253 = ADVANCED_FACE ( 'NONE', ( #2082 ), #1826, .F. ) ;
#254 = CARTESIAN_POINT ( 'NONE',  ( 3.061616997868384127E-16, -67.50000000000000000, 2.500000000000000444 ) ) ;
#255 = CARTESIAN_POINT ( 'NONE',  ( -0.2999999999999999889, -119.0796226588036717, -0.7373253218603728065 ) ) ;
#256 = SURFACE_SIDE_STYLE ('',( #1538 ) ) ;
#257 = CARTESIAN_POINT ( 'NONE',  ( 0.000000000000000000, -125.0000000000000000, 0.000000000000000000 ) ) ;
#258 = CARTESIAN_POINT ( 'NONE',  ( -8.596526774713705521, -52.79999999999999716, 0.2821220414048196123 ) ) ;
#259 = AXIS2_PLACEMENT_3D ( 'NONE', #2090, #2508, #2767 ) ;
#260 = ORIENTED_EDGE ( 'NONE', *, *, #511, .T. ) ;
#261 = PRESENTATION_STYLE_ASSIGNMENT (( #498 ) ) ;
#262 = CARTESIAN_POINT ( 'NONE',  ( 1.116875426047833963, -72.24257843717799688, -4.876070537812395855 ) ) ;
#263 = AXIS2_PLACEMENT_3D ( 'NONE', #405, #1676, #1708 ) ;
#264 = CARTESIAN_POINT ( 'NONE',  ( -7.500000000000000000, 0.000000000000000000, -10.00000000000000000 ) ) ;
#265 = CARTESIAN_POINT ( 'NONE',  ( -0.6766787981060014001, -7.476722154948000743, 4.965272001127371659 ) ) ;
#266 = AXIS2_PLACEMENT_3D ( 'NONE', #564, #2546, #2299 ) ;
#267 = ORIENTED_EDGE ( 'NONE', *, *, #2329, .T. ) ;
#268 = CARTESIAN_POINT ( 'NONE',  ( 5.000001686767464371, -51.50000562255823411, -0.09877180560914068652 ) ) ;
#269 = CARTESIAN_POINT ( 'NONE',  ( -4.325820249441205689, -65.83546891105626742, 2.526170042365371682 ) ) ;
#270 = CARTESIAN_POINT ( 'NONE',  ( -4.793520869840776299, -50.48574331923479264, -1.422568331971221456 ) ) ;
#271 = FACE_OUTER_BOUND ( 'NONE', #2659, .T. ) ;
#272 = DIRECTION ( 'NONE',  ( 1.000000000000000000, -0.000000000000000000, -0.000000000000000000 ) ) ;
#273 = EDGE_CURVE ( 'NONE', #2217, #3170, #1026, .T. ) ;
#274 = CARTESIAN_POINT ( 'NONE',  ( 8.564669657331105412, -50.44377267524160402, 1.332368788789859204 ) ) ;
#275 = B_SPLINE_CURVE_WITH_KNOTS ( 'NONE', 3,
 ( #1048, #3032, #3021, #3050, #255, #1250 ),
 .UNSPECIFIED., .F., .F.,
 ( 4, 2, 4 ),
 ( 0.0004720815379052809273, 0.0007077329675634635737, 0.0009433843972216461116 ),
 .UNSPECIFIED. ) ;
#276 = CARTESIAN_POINT ( 'NONE',  ( -8.599999999999996092, -50.00000000000000000, -0.5466666666666361030 ) ) ;
#277 = VERTEX_POINT ( 'NONE', #596 ) ;
#278 =( NAMED_UNIT ( * ) PLANE_ANGLE_UNIT ( ) SI_UNIT ( $, .RADIAN. ) );
#279 = APPLICATION_CONTEXT ( 'automotive_design' ) ;
#280 = ADVANCED_FACE ( 'NONE', ( #1859 ), #1120, .F. ) ;
#281 = CARTESIAN_POINT ( 'NONE',  ( 0.000000000000000000, -7.500000000000000000, 4.999999999999999112 ) ) ;
#282 = CARTESIAN_POINT ( 'NONE',  ( -7.500000000000000888, 30.00000000000000000, 18.00000000000000355 ) ) ;
#283 = ORIENTED_EDGE ( 'NONE', *, *, #618, .F. ) ;
#284 = CARTESIAN_POINT ( 'NONE',  ( 4.769696007084729850, -50.00000000000000000, 1.499999999999994449 ) ) ;
#285 = CARTESIAN_POINT ( 'NONE',  ( -2.982843918280285944, -47.20000000000001705, 11.10373667793902541 ) ) ;
#286 = ORIENTED_EDGE ( 'NONE', *, *, #755, .F. ) ;
#287 = CARTESIAN_POINT ( 'NONE',  ( -4.871328134482659777, -50.99213922289512624, -1.129209473734892777 ) ) ;
#288 = FACE_OUTER_BOUND ( 'NONE', #2430, .T. ) ;
#289 = PLANE ( 'NONE',  #517 ) ;
#290 = DIRECTION ( 'NONE',  ( 1.000000000000000000, 0.000000000000000000, 0.000000000000000000 ) ) ;
#291 = EDGE_CURVE ( 'NONE', #1132, #1384, #2523, .T. ) ;
#292 = CARTESIAN_POINT ( 'NONE',  ( 9.199433601069458177, -51.18229052107441390, 0.7695943483561379361 ) ) ;
#293 = CARTESIAN_POINT ( 'NONE',  ( 8.324422814932070480, -50.00000000000000000, 2.231815450537910639 ) ) ;
#294 = ORIENTED_EDGE ( 'NONE', *, *, #1983, .F. ) ;
#295 = CARTESIAN_POINT ( 'NONE',  ( 2.816687638038912549E-16, -60.00000000000000000, -2.300000000000000266 ) ) ;
#296 = AXIS2_PLACEMENT_3D ( 'NONE', #3015, #539, #1547 ) ;
#297 = EDGE_CURVE ( 'NONE', #2166, #335, #90, .T. ) ;
#298 = CARTESIAN_POINT ( 'NONE',  ( -0.1568842751130637148, -119.2672622186050262, 0.7728910312014006800 ) ) ;
#299 = CARTESIAN_POINT ( 'NONE',  ( -7.500000000000000000, -50.00000000000000000, 1.499999999999994449 ) ) ;
#300 = ORIENTED_EDGE ( 'NONE', *, *, #804, .T. ) ;
#301 = CARTESIAN_POINT ( 'NONE',  ( 4.977300154039397739, -51.42297266766095021, 0.4847224211361968460 ) ) ;
#302 = CARTESIAN_POINT ( 'NONE',  ( -8.582665138674013150, -47.20000000000001705, 0.5636706063486748297 ) ) ;
#303 = EDGE_CURVE ( 'NONE', #1969, #1046, #611, .T. ) ;
#304 = AXIS2_PLACEMENT_3D ( 'NONE', #1584, #565, #1317 ) ;
#305 = CARTESIAN_POINT ( 'NONE',  ( -4.858119196087239189, -73.52168444273505088, 1.194558663167261781 ) ) ;
#306 = EDGE_CURVE ( 'NONE', #661, #403, #2966, .T. ) ;
#307 = PLANE ( 'NONE',  #836 ) ;
#308 = ORIENTED_EDGE ( 'NONE', *, *, #2329, .F. ) ;
#309 = CARTESIAN_POINT ( 'NONE',  ( 0.000000000000000000, 0.000000000000000000, 0.000000000000000000 ) ) ;
#310 = CARTESIAN_POINT ( 'NONE',  ( 5.000000000000000000, 5.590169943749473624, 10.00000000000000178 ) ) ;
#311 = CARTESIAN_POINT ( 'NONE',  ( -5.285102517542626721, -50.00000000000000000, 6.877134118847252786 ) ) ;
#312 = EDGE_LOOP ( 'NONE', ( #1653, #125 ) ) ;
#313 = LINE ( 'NONE', #1936, #1957 ) ;
#314 = AXIS2_PLACEMENT_3D ( 'NONE', #858, #1399, #2660 ) ;
#315 = CARTESIAN_POINT ( 'NONE',  ( -8.599996472200352571, -50.00000000000000000, 0.1525981975067654262 ) ) ;
#316 = CARTESIAN_POINT ( 'NONE',  ( 2.500000000000004441, -71.46446609406727646, -1.464466094067262025 ) ) ;
#317 = ORIENTED_EDGE ( 'NONE', *, *, #2514, .F. ) ;
#318 = AXIS2_PLACEMENT_3D ( 'NONE', #2727, #459, #1218 ) ;
#319 = CARTESIAN_POINT ( 'NONE',  ( 4.985720285031673527, -51.45180769512853658, -0.3898302721915644087 ) ) ;
#320 = EDGE_CURVE ( 'NONE', #1146, #2520, #1308, .T. ) ;
#321 = CARTESIAN_POINT ( 'NONE',  ( -8.596526774713705521, -47.20000000000001705, 0.2821220414048196123 ) ) ;
#322 = PRESENTATION_LAYER_ASSIGNMENT (  '', '', ( #2798 ) ) ;
#323 = ORIENTED_EDGE ( 'NONE', *, *, #1391, .F. ) ;
#324 = CARTESIAN_POINT ( 'NONE',  ( -4.769696007084725409, -50.00000000000000000, -1.500000000000006439 ) ) ;
#325 = DIRECTION ( 'NONE',  ( 1.000000000000000000, 0.000000000000000000, 0.000000000000000000 ) ) ;
#326 = ORIENTED_EDGE ( 'NONE', *, *, #1477, .F. ) ;
#327 = FILL_AREA_STYLE ('',( #2835 ) ) ;
#328 = CARTESIAN_POINT ( 'NONE',  ( 2.500000000000008438, -70.00000000000000000, -4.330127018922187432 ) ) ;
#329 = CARTESIAN_POINT ( 'NONE',  ( 8.599999999999996092, -52.79999999999999716, -1.093333333333372126 ) ) ;
#330 = EDGE_LOOP ( 'NONE', ( #1360, #1445, #1184, #1112, #1617, #2935, #2615, #1831 ) ) ;
#331 = CARTESIAN_POINT ( 'NONE',  ( 0.000000000000000000, -80.00000000000000000, 0.000000000000000000 ) ) ;
#332 = CARTESIAN_POINT ( 'NONE',  ( 4.476439251420855747, 6.019721759973592157, 2.250752599798611975 ) ) ;
#333 = CARTESIAN_POINT ( 'NONE',  ( -1.375028959113679727, -64.14968884627424472, 4.819517586941451270 ) ) ;
#334 = CARTESIAN_POINT ( 'NONE',  ( -4.999999999999999112, 30.00000000000000000, 18.00000000000000355 ) ) ;
#335 = VERTEX_POINT ( 'NONE', #2320 ) ;
#336 = CARTESIAN_POINT ( 'NONE',  ( -4.477156588595653020, 6.019182485879955635, 2.249288964509364774 ) ) ;
#337 = CARTESIAN_POINT ( 'NONE',  ( 4.331939449206418047, -47.20000000000001705, 7.514224851275111305 ) ) ;
#338 = ORIENTED_EDGE ( 'NONE', *, *, #2208, .F. ) ;
#339 = DIRECTION ( 'NONE',  ( -0.000000000000000000, 1.000000000000000000, -0.000000000000000000 ) ) ;
#340 = ADVANCED_FACE ( 'NONE', ( #832 ), #2291, .T. ) ;
#341 = CARTESIAN_POINT ( 'NONE',  ( -5.285102517542626721, -50.00000000000000000, 6.877134118847252786 ) ) ;
#342 = VERTEX_POINT ( 'NONE', #19 ) ;
#343 = CARTESIAN_POINT ( 'NONE',  ( -2.499999999999995559, -70.00000000000000000, 0.000000000000000000 ) ) ;
#344 = CARTESIAN_POINT ( 'NONE',  ( -2.499999999999991118, -70.00000000000000000, 10.00000000000000000 ) ) ;
#345 = CARTESIAN_POINT ( 'NONE',  ( 9.676554491074602637, -48.63437908886126593, 0.3185635799549096925 ) ) ;
#346 = ORIENTED_EDGE ( 'NONE', *, *, #411, .F. ) ;
#347 = EDGE_CURVE ( 'NONE', #1810, #870, #2221, .T. ) ;
#348 = LINE ( 'NONE', #2156, #846 ) ;
#349 = CARTESIAN_POINT ( 'NONE',  ( 3.321910197521175778, 6.728960966335735705, 3.750313380908745664 ) ) ;
#350 = CARTESIAN_POINT ( 'NONE',  ( 4.769696007084729850, -50.00000000000000000, 1.499999999999994449 ) ) ;
#351 = CARTESIAN_POINT ( 'NONE',  ( 6.121942914840092871E-16, -7.500000000000000000, -4.999999999999999112 ) ) ;
#352 = EDGE_LOOP ( 'NONE', ( #2643, #317, #2086, #589 ) ) ;
#353 = LINE ( 'NONE', #1361, #2518 ) ;
#354 = AXIS2_PLACEMENT_3D ( 'NONE', #1287, #2089, #1073 ) ;
#355 = CARTESIAN_POINT ( 'NONE',  ( -11.39999999999999680, -52.79999999999999716, -1.639999999999997460 ) ) ;
#356 = VERTEX_POINT ( 'NONE', #49 ) ;
#357 = PRODUCT ( 'connecting link', 'connecting link', '', ( #2766 ) ) ;
#358 = CARTESIAN_POINT ( 'NONE',  ( -2.499999999999991118, -70.00000000000000000, -4.330127018922196314 ) ) ;
#359 = CARTESIAN_POINT ( 'NONE',  ( 8.572527594031472993E-15, -70.00000000000000000, 10.00000000000000000 ) ) ;
#360 = ORIENTED_EDGE ( 'NONE', *, *, #1553, .T. ) ;
#361 = CARTESIAN_POINT ( 'NONE',  ( 6.122861072698252249E-16, -67.50000000000000000, -4.999999999999999112 ) ) ;
#362 = EDGE_CURVE ( 'NONE', #342, #3130, #37, .T. ) ;
#363 = CARTESIAN_POINT ( 'NONE',  ( 3.061616997868384127E-16, -72.50000000000001421, 2.500000000000000444 ) ) ;
#364 = CARTESIAN_POINT ( 'NONE',  ( 1.985358491602502662, -68.47218767861880906, -4.589996648303077187 ) ) ;
#365 = VERTEX_POINT ( 'NONE', #66 ) ;
#366 = CARTESIAN_POINT ( 'NONE',  ( 0.2999999999999837796, -116.3333797136428132, 0.8840511146466889514 ) ) ;
#367 = CARTESIAN_POINT ( 'NONE',  ( 3.971188403759415397, 6.365899760466498414, 3.054486213830300390 ) ) ;
#368 = CARTESIAN_POINT ( 'NONE',  ( -9.959683570761574956, -47.20000000000001705, 5.743837162464267898 ) ) ;
#369 = CARTESIAN_POINT ( 'NONE',  ( -11.39999999999999680, -50.00000000000000000, -1.400000000000000133 ) ) ;
#370 = CARTESIAN_POINT ( 'NONE',  ( -3.966867482980610315, 6.368676471623262003, 3.060450018115215443 ) ) ;
#371 = AXIS2_PLACEMENT_3D ( 'NONE', #462, #759, #1502 ) ;
#372 = CARTESIAN_POINT ( 'NONE',  ( -11.39999999999999680, -50.00000000000000000, -1.639999999999997460 ) ) ;
#373 = ORIENTED_EDGE ( 'NONE', *, *, #1718, .F. ) ;
#374 = DIRECTION ( 'NONE',  ( 0.000000000000000000, 0.000000000000000000, 1.000000000000000000 ) ) ;
#375 =( GEOMETRIC_REPRESENTATION_CONTEXT ( 3 ) GLOBAL_UNCERTAINTY_ASSIGNED_CONTEXT ( ( #8 ) ) GLOBAL_UNIT_ASSIGNED_CONTEXT ( ( #1107, #1543, #534 ) ) REPRESENTATION_CONTEXT ( 'NONE', 'WORKASPACE' ) );
#376 = ORIENTED_EDGE ( 'NONE', *, *, #347, .F. ) ;
#377 = CARTESIAN_POINT ( 'NONE',  ( 3.061616997868384127E-16, -67.50000000000000000, 2.500000000000000444 ) ) ;
#378 = LINE ( 'NONE', #1386, #2256 ) ;
#379 = CARTESIAN_POINT ( 'NONE',  ( 8.485280282859413603, -50.00000000000000000, 1.400000000000001021 ) ) ;
#380 = ORIENTED_EDGE ( 'NONE', *, *, #362, .T. ) ;
#381 = CARTESIAN_POINT ( 'NONE',  ( 11.39999999999999680, -50.00000000000000000, -1.400000000003877254 ) ) ;
#382 =( LENGTH_UNIT ( ) NAMED_UNIT ( * ) SI_UNIT ( .MILLI., .METRE. ) );
#383 = CARTESIAN_POINT ( 'NONE',  ( -11.30825875096001454, -50.00000000000000000, 1.490875164968288757 ) ) ;
#384 = PRODUCT_DEFINITION_SHAPE ( 'NONE', 'NONE',  #1297 ) ;
#385 = CARTESIAN_POINT ( 'NONE',  ( -3.077296587540346184, -6.845542784947758364, -3.953776968828220717 ) ) ;
#386 = EDGE_CURVE ( 'NONE', #1748, #1911, #3165, .T. ) ;
#387 = CARTESIAN_POINT ( 'NONE',  ( -4.999765607858179806, 5.590379590366716833, 0.3449705472529415728 ) ) ;
#388 = CARTESIAN_POINT ( 'NONE',  ( 11.37702123033534995, -47.20000000000001705, 0.7471912688806705560 ) ) ;
#389 = EDGE_LOOP ( 'NONE', ( #1165, #392, #454 ) ) ;
#390 = CARTESIAN_POINT ( 'NONE',  ( 0.000000000000000000, -72.60000000000000853, 0.000000000000000000 ) ) ;
#391 = APPLICATION_CONTEXT ( 'automotive_design' ) ;
#392 = ORIENTED_EDGE ( 'NONE', *, *, #1084, .F. ) ;
#393 = CARTESIAN_POINT ( 'NONE',  ( 0.2999999999999837796, -118.9999999999982379, 0.7416198487096254954 ) ) ;
#394 = DIRECTION ( 'NONE',  ( -0.000000000000000000, -0.000000000000000000, 1.000000000000000000 ) ) ;
#395 = LINE ( 'NONE', #1155, #422 ) ;
#396 = EDGE_LOOP ( 'NONE', ( #157, #1556, #839, #427 ) ) ;
#397 = CARTESIAN_POINT ( 'NONE',  ( -2.499999999999995559, -70.00000000000000000, 0.000000000000000000 ) ) ;
#398 = CARTESIAN_POINT ( 'NONE',  ( -11.25335008359214584, -47.20000000000001705, 1.860476840075229843 ) ) ;
#399 = CARTESIAN_POINT ( 'NONE',  ( -9.116201041288242379, -50.00000000000000000, 7.005833569791151128 ) ) ;
#400 = CARTESIAN_POINT ( 'NONE',  ( -3.766216509439173965, 6.490735160851770047, 3.303865152441167297 ) ) ;
#401 = EDGE_CURVE ( 'NONE', #2166, #2400, #1852, .T. ) ;
#402 = CARTESIAN_POINT ( 'NONE',  ( -11.37702123033521850, -52.79999999999999716, 0.7471912688805021352 ) ) ;
#403 = VERTEX_POINT ( 'NONE', #2824 ) ;
#404 = AXIS2_PLACEMENT_3D ( 'NONE', #2772, #2300, #1519 ) ;
#405 = CARTESIAN_POINT ( 'NONE',  ( 0.000000000000000000, -84.99999999999998579, 0.000000000000000000 ) ) ;
#406 = CARTESIAN_POINT ( 'NONE',  ( 4.865239396163736352, -5.708012565174444219, -1.165122949380803741 ) ) ;
#407 = ADVANCED_FACE ( 'NONE', ( #555 ), #888, .T. ) ;
#408 = AXIS2_PLACEMENT_3D ( 'NONE', #2455, #735, #1193 ) ;
#409 = ORIENTED_EDGE ( 'NONE', *, *, #362, .F. ) ;
#410 = FILL_AREA_STYLE ('',( #1878 ) ) ;
#411 = EDGE_CURVE ( 'NONE', #1093, #651, #145, .T. ) ;
#412 = DIRECTION ( 'NONE',  ( -0.000000000000000000, -0.000000000000000000, -1.000000000000000000 ) ) ;
#413 = CARTESIAN_POINT ( 'NONE',  ( 1.541913646847672403, -68.00584954049281805, -4.762550599683263108 ) ) ;
#414 = ORIENTED_EDGE ( 'NONE', *, *, #995, .T. ) ;
#415 = AXIS2_PLACEMENT_3D ( 'NONE', #572, #1274, #519 ) ;
#416 = CARTESIAN_POINT ( 'NONE',  ( -4.871117609892888112, -49.00886260987331866, 1.130144156083558560 ) ) ;
#417 = CARTESIAN_POINT ( 'NONE',  ( -11.25335008359228794, -50.00000000000000000, 1.860476840075229621 ) ) ;
#418 = CARTESIAN_POINT ( 'NONE',  ( -1.654328459400600471, -7.322002074975777930, -4.729864656991090932 ) ) ;
#419 = CARTESIAN_POINT ( 'NONE',  ( 0.07897820435409852458, -119.2999999999982350, -0.7850000000000507683 ) ) ;
#420 = CARTESIAN_POINT ( 'NONE',  ( 11.39999999999999680, -50.00000000000000000, -0.5466666666666269991 ) ) ;
#421 = ORIENTED_EDGE ( 'NONE', *, *, #2954, .T. ) ;
#422 = VECTOR ( 'NONE', #2170, 1000.000000000000000 ) ;
#423 = CARTESIAN_POINT ( 'NONE',  ( -2.250215587473127332, -50.00000000000000000, 8.376503107917878665 ) ) ;
#424 = APPLICATION_PROTOCOL_DEFINITION ( 'draft international standard', 'automotive_design', 1998, #1465 ) ;
#425 =( GEOMETRIC_REPRESENTATION_CONTEXT ( 3 ) GLOBAL_UNCERTAINTY_ASSIGNED_CONTEXT ( ( #2296 ) ) GLOBAL_UNIT_ASSIGNED_CONTEXT ( ( #2905, #1350, #613 ) ) REPRESENTATION_CONTEXT ( 'NONE', 'WORKASPACE' ) );
#426 = CARTESIAN_POINT ( 'NONE',  ( 3.326284669807233918, -6.726800191391157924, -3.746459129603366467 ) ) ;
#427 = ORIENTED_EDGE ( 'NONE', *, *, #952, .F. ) ;
#428 = CARTESIAN_POINT ( 'NONE',  ( 3.982914377913047144, -65.50635683910327600, 3.038300766938665465 ) ) ;
#429 = CARTESIAN_POINT ( 'NONE',  ( -8.599999999999996092, -50.00000000000000000, -1.366666666666159768 ) ) ;
#430 = DIRECTION ( 'NONE',  ( 0.000000000000000000, 1.000000000000000000, 0.000000000000000000 ) ) ;
#431 = MECHANICAL_DESIGN_GEOMETRIC_PRESENTATION_REPRESENTATION (  '', ( #1645 ), #485 ) ;
#432 = CARTESIAN_POINT ( 'NONE',  ( 1.698458751326837435, -75.76378408612910675, 4.714595771049563844 ) ) ;
#433 = EDGE_CURVE ( 'NONE', #1583, #67, #2738, .T. ) ;
#434 = CARTESIAN_POINT ( 'NONE',  ( -4.828119302692784665, -49.24690690879460675, -1.300931117799746906 ) ) ;
#435 = CARTESIAN_POINT ( 'NONE',  ( -11.39999532361432522, -47.20000000000001705, 0.1755699507458657049 ) ) ;
#436 = CARTESIAN_POINT ( 'NONE',  ( -2.982843918280285944, -50.00000000000000000, 11.10373667793902541 ) ) ;
#437 = DIRECTION ( 'NONE',  ( -1.000000000000000000, 0.000000000000000000, 0.000000000000000000 ) ) ;
#438 = CARTESIAN_POINT ( 'NONE',  ( -7.005833569766191538, -52.79999999999999716, 9.116201041262108618 ) ) ;
#439 = VERTEX_POINT ( 'NONE', #282 ) ;
#440 = CARTESIAN_POINT ( 'NONE',  ( -8.324422814933019055, -50.00000000000000000, 2.231815450536601464 ) ) ;
#441 = CARTESIAN_POINT ( 'NONE',  ( 1.654531499027267483, -71.88102071354902023, -4.719874665594111285 ) ) ;
#442 = B_SPLINE_CURVE_WITH_KNOTS ( 'NONE', 3,
 ( #718, #1688, #959, #703, #2705, #1441 ),
 .UNSPECIFIED., .F., .F.,
 ( 4, 2, 4 ),
 ( 0.0004738143657684039823, 0.0007102755844724215365, 0.0009467368031764390908 ),
 .UNSPECIFIED. ) ;
#443 = FACE_OUTER_BOUND ( 'NONE', #2382, .T. ) ;
#444 = ORIENTED_EDGE ( 'NONE', *, *, #386, .F. ) ;
#445 = DIRECTION ( 'NONE',  ( 1.000000000000000000, 0.000000000000000000, 0.000000000000000000 ) ) ;
#446 = CARTESIAN_POINT ( 'NONE',  ( 5.285102517541700351, -50.00000000000000000, 6.877134118846478295 ) ) ;
#447 = CARTESIAN_POINT ( 'NONE',  ( -2.499999999999999556, 3.061616997868382648E-16, 10.00000000000000000 ) ) ;
#448 = CARTESIAN_POINT ( 'NONE',  ( 0.1739454948912135535, -76.00000000000001421, 4.999999999999999112 ) ) ;
#449 = CARTESIAN_POINT ( 'NONE',  ( -4.769696007084725409, -49.90029503198832828, -1.500000000000006217 ) ) ;
#450 = CARTESIAN_POINT ( 'NONE',  ( 11.36325033731725576, -52.79999999999999716, 0.9334869871343942638 ) ) ;
#451 = CARTESIAN_POINT ( 'NONE',  ( 11.39999999999999680, -50.00000000000000000, -1.013333333334534458 ) ) ;
#452 = CARTESIAN_POINT ( 'NONE',  ( -11.38628138490143371, -50.22360298513551413, -1.386281384901433045 ) ) ;
#453 = CARTESIAN_POINT ( 'NONE',  ( 11.40000778997679198, -52.79999999999999716, -0.2924664341912773247 ) ) ;
#454 = ORIENTED_EDGE ( 'NONE', *, *, #1643, .F. ) ;
#455 = CARTESIAN_POINT ( 'NONE',  ( -8.600005876649037262, -47.20000000000001705, -0.2541998246238979520 ) ) ;
#456 = CARTESIAN_POINT ( 'NONE',  ( 1.653246020961511187, -7.322320024462306343, -4.730368990601279577 ) ) ;
#457 = SHAPE_REPRESENTATION ( 'Needle Bar', ( #1692 ), #1164 ) ;
#458 = ORIENTED_EDGE ( 'NONE', *, *, #1898, .F. ) ;
#459 = DIRECTION ( 'NONE',  ( 0.000000000000000000, 0.000000000000000000, 1.000000000000000000 ) ) ;
#460 =( GEOMETRIC_REPRESENTATION_CONTEXT ( 3 ) GLOBAL_UNCERTAINTY_ASSIGNED_CONTEXT ( ( #236 ) ) GLOBAL_UNIT_ASSIGNED_CONTEXT ( ( #1255, #1270, #3012 ) ) REPRESENTATION_CONTEXT ( 'NONE', 'WORKASPACE' ) );
#461 = CARTESIAN_POINT ( 'NONE',  ( -5.285102517542626721, -50.00000000000000000, 6.877134118847252786 ) ) ;
#462 = CARTESIAN_POINT ( 'NONE',  ( 0.000000000000000000, 30.00000000000000000, 18.00000000000000355 ) ) ;
#463 = FACE_BOUND ( 'NONE', #2805, .T. ) ;
#464 = EDGE_CURVE ( 'NONE', #1883, #2883, #2843, .T. ) ;
#465 = CARTESIAN_POINT ( 'NONE',  ( -4.985625624127048461, -48.54851733604390773, 0.3909128500499727821 ) ) ;
#466 = VECTOR ( 'NONE', #2091, 1000.000000000000000 ) ;
#467 = CARTESIAN_POINT ( 'NONE',  ( 11.39539595717853082, -50.00000000000000000, 0.3739757293042009212 ) ) ;
#468 = CARTESIAN_POINT ( 'NONE',  ( 4.999974214802088035, -48.50008595066712047, -0.1976414581757740541 ) ) ;
#469 = CARTESIAN_POINT ( 'NONE',  ( 0.000000000000000000, 30.00000000000000000, 18.00000000000000355 ) ) ;
#470 = CARTESIAN_POINT ( 'NONE',  ( 8.599999999999996092, -52.79999999999999716, -1.639999999999997460 ) ) ;
#471 = ORIENTED_EDGE ( 'NONE', *, *, #568, .F. ) ;
#472 = CARTESIAN_POINT ( 'NONE',  ( -1.125736483477000061, -47.20000000000001705, 8.599999999999996092 ) ) ;
#473 = EDGE_CURVE ( 'NONE', #1139, #1195, #1896, .T. ) ;
#474 = CARTESIAN_POINT ( 'NONE',  ( 10.15784101500072190, -48.59999999999998010, -0.1578371243778893540 ) ) ;
#475 = CARTESIAN_POINT ( 'NONE',  ( 0.000000000000000000, 30.00000000000000000, 10.00000000000000000 ) ) ;
#476 = VECTOR ( 'NONE', #2544, 1000.000000000000000 ) ;
#477 = CARTESIAN_POINT ( 'NONE',  ( 8.160064090060387798, -47.20000000000001705, 2.773119917860402239 ) ) ;
#478 = DIRECTION ( 'NONE',  ( 1.000000000000000000, 0.000000000000000000, 0.000000000000000000 ) ) ;
#479 = DIRECTION ( 'NONE',  ( 0.000000000000000000, 0.000000000000000000, 1.000000000000000000 ) ) ;
#480=STYLED_ITEM('',(#3321),#2670);
#481 = CARTESIAN_POINT ( 'NONE',  ( 9.838268070989578007, -51.39301687163384003, 0.1607570464466796800 ) ) ;
#482 = EDGE_CURVE ( 'NONE', #1748, #2258, #2467, .T. ) ;
#483 = CARTESIAN_POINT ( 'NONE',  ( -7.005833569766191538, -52.79999999999999716, 9.116201041262108618 ) ) ;
#484 = CARTESIAN_POINT ( 'NONE',  ( 11.25335008359272493, -50.00000000000000000, 1.860476840074170246 ) ) ;
#485 =( GEOMETRIC_REPRESENTATION_CONTEXT ( 3 ) GLOBAL_UNCERTAINTY_ASSIGNED_CONTEXT ( ( #770 ) ) GLOBAL_UNIT_ASSIGNED_CONTEXT ( ( #75, #3051, #1811 ) ) REPRESENTATION_CONTEXT ( 'NONE', 'WORKASPACE' ) );
#486 = CARTESIAN_POINT ( 'NONE',  ( 8.572527594031472993E-15, -70.00000000000000000, 0.000000000000000000 ) ) ;
#487 = CARTESIAN_POINT ( 'NONE',  ( 5.742338339644331491, -52.79999999999999716, 9.960716663318304853 ) ) ;
#488 = ORIENTED_EDGE ( 'NONE', *, *, #2125, .F. ) ;
#489 = CARTESIAN_POINT ( 'NONE',  ( 2.250215587473118450, -47.20000000000001705, 8.376503107919017310 ) ) ;
#490 = CARTESIAN_POINT ( 'NONE',  ( -3.984264206898689320, -65.50759766373489867, 3.036427941355733129 ) ) ;
#491 = MANIFOLD_SOLID_BREP ( 'Cut-Extrude2', #1303 ) ;
#492 = LINE ( 'NONE', #1970, #1319 ) ;
#493 = CARTESIAN_POINT ( 'NONE',  ( -11.16040725319408011, -49.19031162998081186, -1.160407253194084332 ) ) ;
#494 = CARTESIAN_POINT ( 'NONE',  ( 4.999999999999999112, -73.31662479035543356, 0.3546751931833549421 ) ) ;
#495 = CARTESIAN_POINT ( 'NONE',  ( 2.500000000000000000, 3.061616997868383141E-16, -10.00000000000000000 ) ) ;
#496 = CARTESIAN_POINT ( 'NONE',  ( 10.81682914263883610, -50.00000000000000000, 3.675996170187548540 ) ) ;
#497 = CARTESIAN_POINT ( 'NONE',  ( 4.916101592540525367, -48.80164085375129446, -0.9229043554563169938 ) ) ;
#498 = SURFACE_STYLE_USAGE ( .BOTH. , #227 ) ;
#499 = CARTESIAN_POINT ( 'NONE',  ( -8.582665138674013150, -52.79999999999999716, 0.5636706063486748297 ) ) ;
#500 = EDGE_LOOP ( 'NONE', ( #2350, #616 ) ) ;
#501 = CARTESIAN_POINT ( 'NONE',  ( -0.1574018113688476495, -114.7330607081729994, -1.002653532495389355 ) ) ;
#502 = APPLICATION_PROTOCOL_DEFINITION ( 'draft international standard', 'automotive_design', 1998, #2486 ) ;
#503 = FACE_OUTER_BOUND ( 'NONE', #2122, .T. ) ;
#504 = B_SPLINE_CURVE_WITH_KNOTS ( 'NONE', 3,
 ( #533, #2255, #3074, #2563 ),
 .UNSPECIFIED., .F., .F.,
 ( 4, 4 ),
 ( 0.005008082645073242724, 0.009013720360685706368 ),
 .UNSPECIFIED. ) ;
#505 = CARTESIAN_POINT ( 'NONE',  ( 0.000000000000000000, -60.00000000000000000, 0.000000000000000000 ) ) ;
#506 = PRODUCT_DEFINITION_CONTEXT ( 'detailed design', #1636, 'design' ) ;
#507 = EDGE_CURVE ( 'NONE', #890, #1696, #1738, .T. ) ;
#508 = LINE ( 'NONE', #2045, #3059 ) ;
#509 = CARTESIAN_POINT ( 'NONE',  ( -1.181079518071022826E-19, -76.00000000000001421, 4.999999999999999112 ) ) ;
#510 = CIRCLE ( 'NONE', #354, 6.000000000000001776 ) ;
#511 = EDGE_CURVE ( 'NONE', #810, #1748, #1991, .T. ) ;
#512 = DIRECTION ( 'NONE',  ( 0.000000000000000000, -0.000000000000000000, 1.000000000000000000 ) ) ;
#513 = CARTESIAN_POINT ( 'NONE',  ( -8.599999999999996092, -52.79999999999999716, -1.093333333333363022 ) ) ;
#514 = ORIENTED_EDGE ( 'NONE', *, *, #1474, .T. ) ;
#515 = FACE_BOUND ( 'NONE', #2326, .T. ) ;
#516 = DIRECTION ( 'NONE',  ( 0.000000000000000000, -1.000000000000000000, 0.000000000000000000 ) ) ;
#517 = AXIS2_PLACEMENT_3D ( 'NONE', #2283, #2527, #2034 ) ;
#518 = CARTESIAN_POINT ( 'NONE',  ( 3.950486495955891025E-15, -119.2999999999982776, 0.7850000000000663114 ) ) ;
#519 = DIRECTION ( 'NONE',  ( 0.000000000000000000, 0.000000000000000000, 1.000000000000000000 ) ) ;
#520 = EDGE_LOOP ( 'NONE', ( #2673, #606, #711, #2356 ) ) ;
#521 = AXIS2_PLACEMENT_3D ( 'NONE', #2241, #3247, #2254 ) ;
#522 = LINE ( 'NONE', #2811, #2995 ) ;
#523 = ITEM_DEFINED_TRANSFORMATION ( 'NONE', 'NONE', #2391,  #1692 ) ;
#524 = CARTESIAN_POINT ( 'NONE',  ( 4.999765607858179806, -5.590379590366716833, 0.3449705472529415728 ) ) ;
#525 = CARTESIAN_POINT ( 'NONE',  ( -4.793458659903279795, -50.48507481733130220, 1.422772306546142174 ) ) ;
#526 = CARTESIAN_POINT ( 'NONE',  ( -10.15784101513766835, -48.60000000000000853, -0.1578371242409689901 ) ) ;
#527 = FACE_OUTER_BOUND ( 'NONE', #1943, .T. ) ;
#528 = EDGE_CURVE ( 'NONE', #3170, #1333, #442, .T. ) ;
#529 = AXIS2_PLACEMENT_3D ( 'NONE', #1204, #430, #176 ) ;
#530 = CARTESIAN_POINT ( 'NONE',  ( 9.999999999999989342, -51.39999999999999147, -1.084199742081416524E-20 ) ) ;
#531 = CARTESIAN_POINT ( 'NONE',  ( 8.530791689320604831, -50.00000000000000000, 1.124695299888175182 ) ) ;
#532 = ORIENTED_EDGE ( 'NONE', *, *, #297, .T. ) ;
#533 = CARTESIAN_POINT ( 'NONE',  ( -0.3000000000000161982, -118.9999999999982379, -0.7416198487096117287 ) ) ;
#534 =( NAMED_UNIT ( * ) SI_UNIT ( $, .STERADIAN. ) SOLID_ANGLE_UNIT ( ) );
#535 = CARTESIAN_POINT ( 'NONE',  ( 0.000000000000000000, 0.000000000000000000, -10.00000000000000000 ) ) ;
#536 = PRODUCT_RELATED_PRODUCT_CATEGORY ( 'part', '', ( #862 ) ) ;
#537 = CARTESIAN_POINT ( 'NONE',  ( 0.000000000000000000, -7.500000000000000000, 4.999999999999999112 ) ) ;
#538 = ORIENTED_EDGE ( 'NONE', *, *, #3138, .T. ) ;
#539 = DIRECTION ( 'NONE',  ( -0.000000000000000000, -0.000000000000000000, -1.000000000000000000 ) ) ;
#540 = CARTESIAN_POINT ( 'NONE',  ( -11.25335008359214584, -47.20000000000001705, 1.860476840075229843 ) ) ;
#541 = CARTESIAN_POINT ( 'NONE',  ( 0.000000000000000000, -80.00000000000000000, 4.999999999999999112 ) ) ;
#542 = UNCERTAINTY_MEASURE_WITH_UNIT (LENGTH_MEASURE( 1.000000000000000082E-05 ), #1083, 'distance_accuracy_value', 'NONE');
#543 = CARTESIAN_POINT ( 'NONE',  ( 0.000000000000000000, -60.00000000000000000, 0.000000000000000000 ) ) ;
#544 = CARTESIAN_POINT ( 'NONE',  ( 2.500000000000008882, -70.00000000000000000, 10.00000000000000000 ) ) ;
#545 = SHAPE_REPRESENTATION ( 'MAS-169', ( #2124, #266, #1117, #2391, #955 ), #2280 ) ;
#546 = DIRECTION ( 'NONE',  ( 1.000000000000000000, 0.000000000000000000, 0.000000000000000000 ) ) ;
#547 = EDGE_CURVE ( 'NONE', #2574, #3000, #1416, .T. ) ;
#548 = LINE ( 'NONE', #2266, #1038 ) ;
#549 = CARTESIAN_POINT ( 'NONE',  ( -8.324422814933019055, -52.79999999999999716, 2.231815450536601020 ) ) ;
#550 = ORIENTED_EDGE ( 'NONE', *, *, #1924, .F. ) ;
#551 = SURFACE_STYLE_USAGE ( .BOTH. , #1304 ) ;
#552 = SHAPE_REPRESENTATION_RELATIONSHIP ( 'NONE' , 'NONE' ,  #3271, #2473 ) ;
#553 = EDGE_CURVE ( 'NONE', #2101, #2520, #232, .T. ) ;
#554 = CARTESIAN_POINT ( 'NONE',  ( 8.599999999999996092, -50.00000000000000000, -0.5466666666666269991 ) ) ;
#555 = FACE_OUTER_BOUND ( 'NONE', #1877, .T. ) ;
#556 = ORIENTED_EDGE ( 'NONE', *, *, #2233, .T. ) ;
#557 = CARTESIAN_POINT ( 'NONE',  ( 6.121942914840092871E-16, -7.500000000000000000, -4.999999999999999112 ) ) ;
#558 = EDGE_CURVE ( 'NONE', #1156, #900, #2476, .T. ) ;
#559 = CARTESIAN_POINT ( 'NONE',  ( -11.30825875096015665, -47.20000000000001705, 1.490875164968288979 ) ) ;
#560 = ORIENTED_EDGE ( 'NONE', *, *, #1874, .F. ) ;
#561 = DIRECTION ( 'NONE',  ( 1.000000000000000000, 0.000000000000000000, 0.000000000000000000 ) ) ;
#562 = CARTESIAN_POINT ( 'NONE',  ( -2.300000000000000266, -67.40000000000000568, -1.734723475976807094E-15 ) ) ;
#563 = EDGE_LOOP ( 'NONE', ( #962, #2420, #624, #283 ) ) ;
#564 = CARTESIAN_POINT ( 'NONE',  ( 0.000000000000000000, 0.000000000000000000, 0.000000000000000000 ) ) ;
#565 = DIRECTION ( 'NONE',  ( -0.000000000000000000, -0.000000000000000000, -1.000000000000000000 ) ) ;
#566 = CARTESIAN_POINT ( 'NONE',  ( 8.599999999999996092, -52.79999999999999716, -0.5466666666666269991 ) ) ;
#567 = ORIENTED_EDGE ( 'NONE', *, *, #2749, .F. ) ;
#568 = EDGE_CURVE ( 'NONE', #2400, #3266, #1678, .T. ) ;
#569 = LINE ( 'NONE', #1321, #2226 ) ;
#570 = AXIS2_PLACEMENT_3D ( 'NONE', #1402, #1971, #953 ) ;
#571 = CARTESIAN_POINT ( 'NONE',  ( 1.125736483476999839, -50.00000000000000000, 8.599999999999996092 ) ) ;
#572 = CARTESIAN_POINT ( 'NONE',  ( 0.000000000000000000, -80.00000000000000000, 0.000000000000000000 ) ) ;
#573 = ORIENTED_EDGE ( 'NONE', *, *, #1778, .F. ) ;
#574 = CARTESIAN_POINT ( 'NONE',  ( 4.916186798144710934, -51.19881560760884298, 0.9225820817148873143 ) ) ;
#575 = CARTESIAN_POINT ( 'NONE',  ( 10.81682914263912210, -47.20000000000001705, 3.675996170187548540 ) ) ;
#576 = EDGE_LOOP ( 'NONE', ( #2530, #2251, #199, #247, #1827, #3157, #1316, #88 ) ) ;
#577 = CARTESIAN_POINT ( 'NONE',  ( -4.945777185212984151, -51.30992422645292805, -0.7564652374250301348 ) ) ;
#578 = CARTESIAN_POINT ( 'NONE',  ( 0.000000000000000000, 30.00000000000000000, 18.00000000000000355 ) ) ;
#579 = ORIENTED_EDGE ( 'NONE', *, *, #2417, .F. ) ;
#580 = DIRECTION ( 'NONE',  ( 0.000000000000000000, 1.000000000000000000, 0.000000000000000000 ) ) ;
#581 = CARTESIAN_POINT ( 'NONE',  ( 8.600005876649037262, -52.79999999999999716, -0.2541998246239300374 ) ) ;
#582 = ORIENTED_EDGE ( 'NONE', *, *, #2260, .F. ) ;
#583 = AXIS2_PLACEMENT_3D ( 'NONE', #2757, #3243, #478 ) ;
#584 = DIRECTION ( 'NONE',  ( -0.000000000000000000, -0.000000000000000000, -1.000000000000000000 ) ) ;
#585 = VECTOR ( 'NONE', #739, 1000.000000000000000 ) ;
#586 = CARTESIAN_POINT ( 'NONE',  ( 4.956114419722681852, 5.629162412197389109, 0.6822959203856070465 ) ) ;
#587 = CARTESIAN_POINT ( 'NONE',  ( -2.594030646330689915, -64.58156784093502267, 4.286313293421136983 ) ) ;
#588 = DIRECTION ( 'NONE',  ( 0.000000000000000000, 0.000000000000000000, -1.000000000000000000 ) ) ;
#589 = ORIENTED_EDGE ( 'NONE', *, *, #2208, .T. ) ;
#590 = STYLED_ITEM ( 'NONE', ( #1305 ), #3218 ) ;
#591 = CARTESIAN_POINT ( 'NONE',  ( -3.071765256614000794, 6.848070662608381376, 3.958153484541630629 ) ) ;
#592 = EDGE_CURVE ( 'NONE', #3036, #1621, #1344, .T. ) ;
#593 = CARTESIAN_POINT ( 'NONE',  ( -8.599999999999996092, -47.20000000000001705, -1.093333333333363022 ) ) ;
#594 = PRODUCT_DEFINITION_FORMATION_WITH_SPECIFIED_SOURCE ( 'ANY', '', #654, .NOT_KNOWN. ) ;
#595 = CARTESIAN_POINT ( 'NONE',  ( 0.000000000000000000, 0.000000000000000000, 10.00000000000000000 ) ) ;
#596 = CARTESIAN_POINT ( 'NONE',  ( 2.300000000000000266, -67.40000000000000568, -1.734723475976807094E-15 ) ) ;
#597 = EDGE_LOOP ( 'NONE', ( #2359, #1846, #1716, #2737 ) ) ;
#598 = CARTESIAN_POINT ( 'NONE',  ( -2.369138637566329475, -69.18494310611589526, -4.403673215483854264 ) ) ;
#599 = DIRECTION ( 'NONE',  ( -1.000000000000000000, 0.000000000000000000, -0.000000000000000000 ) ) ;
#600 = CARTESIAN_POINT ( 'NONE',  ( 8.160064090060387798, -50.00000000000000000, 2.773119917860402239 ) ) ;
#601 = ORIENTED_EDGE ( 'NONE', *, *, #1816, .F. ) ;
#602 = CARTESIAN_POINT ( 'NONE',  ( -2.499999999999995559, -70.00000000000000000, 0.000000000000000000 ) ) ;
#603 = CARTESIAN_POINT ( 'NONE',  ( 3.769434200324356166, 6.488926209160664094, -3.300387065219955840 ) ) ;
#604 = CARTESIAN_POINT ( 'NONE',  ( -4.769696007084725409, -50.00000000000000000, -1.500000000000006439 ) ) ;
#605 = PRESENTATION_STYLE_ASSIGNMENT (( #882 ) ) ;
#606 = ORIENTED_EDGE ( 'NONE', *, *, #161, .T. ) ;
#607 = CARTESIAN_POINT ( 'NONE',  ( -2.262527220957939456, 7.157552900320828471, -4.471083064257649120 ) ) ;
#608 = CARTESIAN_POINT ( 'NONE',  ( 11.36325033731732503, -50.00000000000000000, 0.9334869871343942638 ) ) ;
#609 = ADVANCED_FACE ( 'NONE', ( #224 ), #792, .T. ) ;
#610 = CARTESIAN_POINT ( 'NONE',  ( -9.920079092145705602, -48.60000000000000142, 0.07989781697764072876 ) ) ;
#611 = LINE ( 'NONE', #73, #1572 ) ;
#612 = ORIENTED_EDGE ( 'NONE', *, *, #2025, .F. ) ;
#613 =( NAMED_UNIT ( * ) SI_UNIT ( $, .STERADIAN. ) SOLID_ANGLE_UNIT ( ) );
#614 = CARTESIAN_POINT ( 'NONE',  ( -0.3000000000000161982, -118.9999999999982379, -2.300000000000000266 ) ) ;
#615 = DIRECTION ( 'NONE',  ( 0.000000000000000000, 0.000000000000000000, 1.000000000000000000 ) ) ;
#616 = ORIENTED_EDGE ( 'NONE', *, *, #136, .F. ) ;
#617 = ADVANCED_BREP_SHAPE_REPRESENTATION ( '', ( #1595, #1692 ), #2651 ) ;
#618 = EDGE_CURVE ( 'NONE', #1320, #3085, #548, .T. ) ;
#619 = CARTESIAN_POINT ( 'NONE',  ( 0.000000000000000000, -84.99999999999998579, 0.000000000000000000 ) ) ;
#620 = FILL_AREA_STYLE_COLOUR ( '', #2179 ) ;
#621 = CARTESIAN_POINT ( 'NONE',  ( 3.078112602769041306, 6.845324219060942461, 3.953457562721318652 ) ) ;
#622 = CARTESIAN_POINT ( 'NONE',  ( 8.599996472200352571, -47.20000000000001705, 0.1525981975067867147 ) ) ;
#623 = CARTESIAN_POINT ( 'NONE',  ( 2.500000000000004441, -70.00000000000000000, 0.000000000000000000 ) ) ;
#624 = ORIENTED_EDGE ( 'NONE', *, *, #2822, .T. ) ;
#625 = CARTESIAN_POINT ( 'NONE',  ( -1.653246020961511187, 7.322320024462306343, -4.730368990601279577 ) ) ;
#626 = PRESENTATION_LAYER_ASSIGNMENT (  '', '', ( #1622 ) ) ;
#627 = CARTESIAN_POINT ( 'NONE',  ( -11.40000778997679198, -52.79999999999999716, -0.2924664341913127408 ) ) ;
#628 = ORIENTED_EDGE ( 'NONE', *, *, #1396, .F. ) ;
#629 = CARTESIAN_POINT ( 'NONE',  ( -9.354236102686607879, -48.73731279115566650, 0.6262106814100150132 ) ) ;
#630 = VECTOR ( 'NONE', #32, 1000.000000000000000 ) ;
#631 = ORIENTED_EDGE ( 'NONE', *, *, #2234, .F. ) ;
#632 = CARTESIAN_POINT ( 'NONE',  ( 0.000000000000000000, -80.00000000000000000, 0.000000000000000000 ) ) ;
#633 = DIRECTION ( 'NONE',  ( 1.000000000000000000, 0.000000000000000000, 0.000000000000000000 ) ) ;
#634 = B_SPLINE_CURVE_WITH_KNOTS ( 'NONE', 3,
 ( #1752, #1800, #1010, #812, #2806, #993 ),
 .UNSPECIFIED., .F., .F.,
 ( 4, 2, 4 ),
 ( 0.0004738143657684043076, 0.0007102755844724216450, 0.0009467368031764393076 ),
 .UNSPECIFIED. ) ;
#635 = CARTESIAN_POINT ( 'NONE',  ( 2.500000000000008438, -70.00000000000000000, -4.330127018922187432 ) ) ;
#636 = ADVANCED_FACE ( 'NONE', ( #1251 ), #2803, .F. ) ;
#637 = ORIENTED_EDGE ( 'NONE', *, *, #1230, .F. ) ;
#638 = CARTESIAN_POINT ( 'NONE',  ( 0.000000000000000000, -84.99999999999998579, 0.000000000000000000 ) ) ;
#639 = CARTESIAN_POINT ( 'NONE',  ( 11.36325033731739609, -47.20000000000001705, 0.9334869871343942638 ) ) ;
#640 = CARTESIAN_POINT ( 'NONE',  ( -0.6733179620838674051, -7.471617105689219329, -4.957340513892267708 ) ) ;
#641 = CARTESIAN_POINT ( 'NONE',  ( -4.481108542057384625, 6.016226048536217341, -2.241414944841849888 ) ) ;
#642 = AXIS2_PLACEMENT_3D ( 'NONE', #1934, #2512, #954 ) ;
#643 = CARTESIAN_POINT ( 'NONE',  ( 11.25335008359272493, -50.00000000000000000, 1.860476840074170246 ) ) ;
#644 = CIRCLE ( 'NONE', #3010, 6.000000000000001776 ) ;
#645 = ORIENTED_EDGE ( 'NONE', *, *, #2417, .T. ) ;
#646 = CARTESIAN_POINT ( 'NONE',  ( -2.369101981968370740, -70.81463507927145429, -4.403671262993352542 ) ) ;
#647 = EDGE_LOOP ( 'NONE', ( #532, #1819 ) ) ;
#648 = CARTESIAN_POINT ( 'NONE',  ( -1.115681787891026344, -67.75684662697969429, -4.876336675329124404 ) ) ;
#649 = CARTESIAN_POINT ( 'NONE',  ( 7.513445500750180805, -50.00000000000000000, 4.333070140107198043 ) ) ;
#650 = CARTESIAN_POINT ( 'NONE',  ( 0.000000000000000000, -80.00000000000000000, 0.000000000000000000 ) ) ;
#651 = VERTEX_POINT ( 'NONE', #2067 ) ;
#652 = ADVANCED_FACE ( 'NONE', ( #1812, #1779, #2515 ), #3022, .T. ) ;
#653 = CARTESIAN_POINT ( 'NONE',  ( -11.40000778997679021, -50.00000000000000000, -0.2924664341913127408 ) ) ;
#654 = PRODUCT ( 'thread guide', 'thread guide', '', ( #1244 ) ) ;
#655 = CARTESIAN_POINT ( 'NONE',  ( -5.000292928619530564, -5.589907940605836956, -0.3348667354298545673 ) ) ;
#656 = DIRECTION ( 'NONE',  ( 1.000000000000000000, 0.000000000000000000, 0.000000000000000000 ) ) ;
#657 = CARTESIAN_POINT ( 'NONE',  ( -11.39539595717866405, -50.00000000000000000, 0.3739757293043588504 ) ) ;
#658 = EDGE_LOOP ( 'NONE', ( #286, #1842 ) ) ;
#659 = ADVANCED_FACE ( 'NONE', ( #2547 ), #1007, .F. ) ;
#660 = CARTESIAN_POINT ( 'NONE',  ( -9.838139443699130737, -48.60697500979578933, 0.1608869294866560606 ) ) ;
#661 = VERTEX_POINT ( 'NONE', #3071 ) ;
#662 = CARTESIAN_POINT ( 'NONE',  ( 0.07888090825136125084, -119.2999999999982066, 0.7850000000000489919 ) ) ;
#663 = CARTESIAN_POINT ( 'NONE',  ( 8.582665138674004268, -50.00000000000000000, 0.5636706063485154017 ) ) ;
#664 = DIRECTION ( 'NONE',  ( -0.000000000000000000, -0.000000000000000000, 1.000000000000000000 ) ) ;
#665 = ORIENTED_EDGE ( 'NONE', *, *, #1677, .T. ) ;
#666 = CARTESIAN_POINT ( 'NONE',  ( -5.000001686767464371, -48.49999437744178010, -0.09877180560914068652 ) ) ;
#667 = CARTESIAN_POINT ( 'NONE',  ( 11.39539595717860188, -47.20000000000001705, 0.3739757293042009767 ) ) ;
#668 = CARTESIAN_POINT ( 'NONE',  ( -1.338285735402328314, -7.387167716089622083, -4.829375120343072147 ) ) ;
#669 = B_SPLINE_CURVE_WITH_KNOTS ( 'NONE', 3,
 ( #1420, #2188, #1387, #2403, #128, #864, #413, #3161, #364, #877, #1172, #2387, #2890, #2922, #1863, #635 ),
 .UNSPECIFIED., .F., .F.,
 ( 4, 2, 2, 2, 2, 2, 2, 4 ),
 ( 0.01192236024948129317, 0.01241818132785782632, 0.01291400240623435947, 0.01390564456298742750, 0.01440146564136396065, 0.01489728671974049554, 0.01539310779811702869, 0.01588892887649356184 ),
 .UNSPECIFIED. ) ;
#670 = DIRECTION ( 'NONE',  ( 0.000000000000000000, 0.000000000000000000, 1.000000000000000000 ) ) ;
#671 = CARTESIAN_POINT ( 'NONE',  ( 11.39999999999999680, -47.20000000000001705, -1.639999999999997460 ) ) ;
#672 = EDGE_CURVE ( 'NONE', #1979, #1630, #2893, .T. ) ;
#673 = EDGE_LOOP ( 'NONE', ( #907, #2695, #45, #2133 ) ) ;
#674 = CARTESIAN_POINT ( 'NONE',  ( 8.572276570257082895, -47.20000000000001705, 0.7042094815225934390 ) ) ;
#675 = VECTOR ( 'NONE', #834, 1000.000000000000000 ) ;
#676 = DIRECTION ( 'NONE',  ( -0.000000000000000000, -0.000000000000000000, -1.000000000000000000 ) ) ;
#677 = DIRECTION ( 'NONE',  ( -1.000000000000000000, 0.000000000000000000, 0.000000000000000000 ) ) ;
#678 = EDGE_LOOP ( 'NONE', ( #784, #1680 ) ) ;
#679 = CARTESIAN_POINT ( 'NONE',  ( 4.815265823182746097, -66.41952955260356362, 1.356348383020189230 ) ) ;
#680 = CARTESIAN_POINT ( 'NONE',  ( 8.599996472200352571, -50.00000000000000000, 0.1525981975067866592 ) ) ;
#681 = CARTESIAN_POINT ( 'NONE',  ( 9.838139443699079223, -48.60697500979577512, 0.1608869294865812039 ) ) ;
#682 = CARTESIAN_POINT ( 'NONE',  ( 9.999999999999989342, -51.39999999999999147, -1.084199742081416524E-20 ) ) ;
#683 = AXIS2_PLACEMENT_3D ( 'NONE', #1844, #891, #876 ) ;
#684 = CARTESIAN_POINT ( 'NONE',  ( -4.871330634494102974, -49.00784869700550672, -1.129198576418441791 ) ) ;
#685 = CARTESIAN_POINT ( 'NONE',  ( 9.116201041286979390, -47.20000000000001705, 7.005833569791843907 ) ) ;
#686 = CARTESIAN_POINT ( 'NONE',  ( 11.39539595717853082, -50.00000000000000000, 0.3739757293042009212 ) ) ;
#687 = CARTESIAN_POINT ( 'NONE',  ( -9.358389811592287444, -51.26439022220001362, 0.6222967749777322810 ) ) ;
#688 = CARTESIAN_POINT ( 'NONE',  ( 8.324422814932072257, -52.79999999999999716, 2.231815450537910195 ) ) ;
#689 = EDGE_LOOP ( 'NONE', ( #1211, #2505, #1101, #92, #1893, #1269, #815, #144, #2074, #1732, #2092 ) ) ;
#690 = CIRCLE ( 'NONE', #791, 2.500000000000000444 ) ;
#691 = CARTESIAN_POINT ( 'NONE',  ( -7.513445500749800665, -50.00000000000000000, 4.333070140105378165 ) ) ;
#692 = EDGE_CURVE ( 'NONE', #67, #3153, #2786, .T. ) ;
#693 = DIRECTION ( 'NONE',  ( 0.000000000000000000, 0.000000000000000000, -1.000000000000000000 ) ) ;
#694 = VERTEX_POINT ( 'NONE', #2035 ) ;
#695 = AXIS2_PLACEMENT_3D ( 'NONE', #124, #1080, #2095 ) ;
#696 = CARTESIAN_POINT ( 'NONE',  ( 0.000000000000000000, 30.00000000000000000, 18.00000000000000355 ) ) ;
#697 = EDGE_CURVE ( 'NONE', #50, #403, #3126, .T. ) ;
#698 = CARTESIAN_POINT ( 'NONE',  ( -2.250215587473127332, -50.00000000000000000, 8.376503107917878665 ) ) ;
#699 = LINE ( 'NONE', #985, #1260 ) ;
#700 = PLANE ( 'NONE',  #2102 ) ;
#701 = CARTESIAN_POINT ( 'NONE',  ( -4.782644271597511043, -49.60515857921176064, 1.460283231774381907 ) ) ;
#702 = CARTESIAN_POINT ( 'NONE',  ( -10.81682914263834405, -52.79999999999999716, 3.675996170188739143 ) ) ;
#703 = CARTESIAN_POINT ( 'NONE',  ( -0.2675651834338630963, -114.8434534129297475, 0.9733310578110722089 ) ) ;
#704 = CARTESIAN_POINT ( 'NONE',  ( -9.838268070989617087, -51.39301687163386134, 0.1607570464467989457 ) ) ;
#705 = CARTESIAN_POINT ( 'NONE',  ( 11.03470001049091032, -52.79999999999999716, 2.958453039085699565 ) ) ;
#706 = ORIENTED_EDGE ( 'NONE', *, *, #196, .F. ) ;
#707 = CARTESIAN_POINT ( 'NONE',  ( 2.250215587473118450, -50.00000000000000000, 8.376503107919017310 ) ) ;
#708 = CARTESIAN_POINT ( 'NONE',  ( 0.000000000000000000, 30.00000000000000000, 18.00000000000000355 ) ) ;
#709 = CARTESIAN_POINT ( 'NONE',  ( 0.000000000000000000, -60.00000000000000000, 0.000000000000000000 ) ) ;
#710 = ADVANCED_FACE ( 'NONE', ( #1300 ), #2316, .F. ) ;
#711 = ORIENTED_EDGE ( 'NONE', *, *, #1884, .T. ) ;
#712 = CYLINDRICAL_SURFACE ( 'NONE', #3063, 1.499999999999999778 ) ;
#713 = FACE_BOUND ( 'NONE', #115, .T. ) ;
#714 = CARTESIAN_POINT ( 'NONE',  ( -5.999999999999992895, -70.00000000000000000, 10.00000000000000000 ) ) ;
#715 = CARTESIAN_POINT ( 'NONE',  ( 9.999999999999989342, -51.39999999999999147, -1.084199742081416524E-20 ) ) ;
#716 = DIRECTION ( 'NONE',  ( -1.000000000000000000, 0.000000000000000000, 0.000000000000000000 ) ) ;
#717 = CARTESIAN_POINT ( 'NONE',  ( 11.30825875096028099, -50.00000000000000000, 1.490875164968454181 ) ) ;
#718 = CARTESIAN_POINT ( 'NONE',  ( -2.347667281524951198E-13, -114.6999999999962228, 1.015000000000727765 ) ) ;
#719 = PLANE ( 'NONE',  #2361 ) ;
#720 = CARTESIAN_POINT ( 'NONE',  ( -8.596526774713705521, -52.79999999999999716, 0.2821220414048196123 ) ) ;
#721 = VERTEX_POINT ( 'NONE', #495 ) ;
#722 = CARTESIAN_POINT ( 'NONE',  ( -7.513445500749801553, -47.20000000000001705, 4.333070140105379942 ) ) ;
#723 = DIRECTION ( 'NONE',  ( -0.000000000000000000, -0.000000000000000000, -1.000000000000000000 ) ) ;
#724 = CARTESIAN_POINT ( 'NONE',  ( 11.40000000000000036, -49.88862030549577042, -1.399999999999994360 ) ) ;
#725 = DIRECTION ( 'NONE',  ( 1.000000000000000000, 0.000000000000000000, 0.000000000000000000 ) ) ;
#726 = CARTESIAN_POINT ( 'NONE',  ( 8.489369361306732031, -47.20000000000001705, 1.403517616196621409 ) ) ;
#727 = CARTESIAN_POINT ( 'NONE',  ( -11.39999999999999680, -50.00000000000000000, -1.400000000000000133 ) ) ;
#728 = CARTESIAN_POINT ( 'NONE',  ( 0.000000000000000000, -125.0000000000000000, 0.4999999999999813483 ) ) ;
#729 = VECTOR ( 'NONE', #820, 1000.000000000000000 ) ;
#730 = CARTESIAN_POINT ( 'NONE',  ( -8.599999999999996092, -50.00000000000000000, -0.5466666666666361030 ) ) ;
#731 = EDGE_CURVE ( 'NONE', #38, #1508, #1891, .T. ) ;
#732 = VECTOR ( 'NONE', #1567, 1000.000000000000000 ) ;
#733 = CARTESIAN_POINT ( 'NONE',  ( 10.81682914263855544, -52.79999999999999716, 3.675996170187548540 ) ) ;
#734 = CARTESIAN_POINT ( 'NONE',  ( 4.769696007084725409, -50.00000000000000000, -1.500000000000006439 ) ) ;
#735 = DIRECTION ( 'NONE',  ( 0.000000000000000000, 1.000000000000000000, 0.000000000000000000 ) ) ;
#736 = CARTESIAN_POINT ( 'NONE',  ( -2.982843918280285944, -52.79999999999999716, 11.10373667793902541 ) ) ;
#737 = ORIENTED_EDGE ( 'NONE', *, *, #2840, .T. ) ;
#738 = CARTESIAN_POINT ( 'NONE',  ( -2.250215587473127332, -47.20000000000001705, 8.376503107917878665 ) ) ;
#739 = DIRECTION ( 'NONE',  ( -0.000000000000000000, -0.000000000000000000, 1.000000000000000000 ) ) ;
#740 = AXIS2_PLACEMENT_3D ( 'NONE', #116, #1623, #2876 ) ;
#741 = DIRECTION ( 'NONE',  ( 0.000000000000000000, 0.000000000000000000, -1.000000000000000000 ) ) ;
#742 = CIRCLE ( 'NONE', #2590, 2.499999999999999556 ) ;
#743 = FACE_BOUND ( 'NONE', #2335, .T. ) ;
#744 = FACE_OUTER_BOUND ( 'NONE', #647, .T. ) ;
#745 = AXIS2_PLACEMENT_3D ( 'NONE', #390, #2344, #2884 ) ;
#746 = B_SPLINE_CURVE_WITH_KNOTS ( 'NONE', 3,
 ( #1376, #2392, #1868, #2638, #2353, #2877, #100, #621, #349, #3113, #367, #3132, #332, #118, #2604, #1109, #586, #867, #1338, #1590, #81, #1090, #2126, #2106, #1850, #2862, #603, #1607, #1357, #3064, #2765, #800, #2275, #1770, #2777, #1577, #1527, #816, #1062, #2075 ),
 .UNSPECIFIED., .F., .F.,
 ( 4, 2, 2, 2, 2, 2, 2, 2, 2, 2, 2, 2, 2, 2, 2, 2, 2, 2, 2, 4 ),
 ( 0.000000000000000000, 0.001009991476537153501, 0.002019982953074307436, 0.003029974429611462239, 0.004039965906148617475, 0.005049957382685771844, 0.006059948859222927947, 0.007069940335760082316, 0.007574936074028659934, 0.008079931812297236685, 0.009089923288834390186, 0.01009991476537154195, 0.01110990624190869892, 0.01211989771844585242, 0.01312988919498300593, 0.01363488493325158528, 0.01413988067152016116, 0.01514987214805731987, 0.01565486788632589749, 0.01615986362459447684 ),
 .UNSPECIFIED. ) ;
#747 = CIRCLE ( 'NONE', #695, 0.4999999999999813483 ) ;
#748 = DIRECTION ( 'NONE',  ( 0.000000000000000000, 0.000000000000000000, -1.000000000000000000 ) ) ;
#749 = CARTESIAN_POINT ( 'NONE',  ( 11.39999999999999680, -52.79999999999999716, -1.639999999999997460 ) ) ;
#750 = CARTESIAN_POINT ( 'NONE',  ( 11.03470001049119453, -50.00000000000000000, 2.958453039085983338 ) ) ;
#751 = EDGE_CURVE ( 'NONE', #2182, #2708, #3107, .T. ) ;
#752 = CARTESIAN_POINT ( 'NONE',  ( -4.331939449206426929, -52.79999999999999716, 7.514224851276242845 ) ) ;
#753 = ORIENTED_EDGE ( 'NONE', *, *, #2111, .F. ) ;
#754 = CARTESIAN_POINT ( 'NONE',  ( 4.945480083184111919, -51.30885859099010560, 0.7590239407556941265 ) ) ;
#755 = EDGE_CURVE ( 'NONE', #3070, #721, #2000, .T. ) ;
#756 = CARTESIAN_POINT ( 'NONE',  ( 1.334319281011194347, -7.387780498848168342, 4.830307711356911504 ) ) ;
#757 = ADVANCED_FACE ( 'NONE', ( #1102 ), #3160, .F. ) ;
#758 = DIRECTION ( 'NONE',  ( 0.000000000000000000, 1.000000000000000000, 0.000000000000000000 ) ) ;
#759 = DIRECTION ( 'NONE',  ( 0.000000000000000000, 0.000000000000000000, 1.000000000000000000 ) ) ;
#760 = DIRECTION ( 'NONE',  ( -0.000000000000000000, 1.000000000000000000, -0.000000000000000000 ) ) ;
#761 = CARTESIAN_POINT ( 'NONE',  ( -2.300000000000000266, -72.60000000000000853, 4.600000000000001421 ) ) ;
#762 = CARTESIAN_POINT ( 'NONE',  ( 1.492255338562904043, -50.00000000000000000, 11.39999999999999680 ) ) ;
#763 = ORIENTED_EDGE ( 'NONE', *, *, #297, .F. ) ;
#764 = LINE ( 'NONE', #2789, #2937 ) ;
#765 = CARTESIAN_POINT ( 'NONE',  ( -8.600005876649037262, -50.00000000000000000, -0.2541998246238979520 ) ) ;
#766 = ORIENTED_EDGE ( 'NONE', *, *, #592, .F. ) ;
#767 = CARTESIAN_POINT ( 'NONE',  ( -0.3000000000000161982, -114.9999999999982236, -0.9539392014169785217 ) ) ;
#768 = CARTESIAN_POINT ( 'NONE',  ( 0.000000000000000000, 0.000000000000000000, 18.00000000000000355 ) ) ;
#769 = CARTESIAN_POINT ( 'NONE',  ( -1.373679055183323117, -75.85067040024597418, 4.819953665648757379 ) ) ;
#770 = UNCERTAINTY_MEASURE_WITH_UNIT (LENGTH_MEASURE( 1.000000000000000082E-05 ), #75, 'distance_accuracy_value', 'NONE');
#771 = CARTESIAN_POINT ( 'NONE',  ( 0.000000000000000000, -125.0000000000000000, 0.000000000000000000 ) ) ;
#772 = FACE_BOUND ( 'NONE', #678, .T. ) ;
#773 =( BOUNDED_CURVE ( )  B_SPLINE_CURVE ( 3, ( #397, #2665, #1405, #2421 ),
 .UNSPECIFIED., .F., .T. ) 
 B_SPLINE_CURVE_WITH_KNOTS ( ( 4, 4 ),
 ( 4.712388980384689674, 6.283185307179586232 ),
 .UNSPECIFIED. ) 
 CURVE ( )  GEOMETRIC_REPRESENTATION_ITEM ( )  RATIONAL_B_SPLINE_CURVE ( ( 1.000000000000000000, 0.8047378541243649375, 0.8047378541243649375, 1.000000000000000000 ) ) 
 REPRESENTATION_ITEM ( '' )  );
#774 = CARTESIAN_POINT ( 'NONE',  ( 0.000000000000000000, 0.000000000000000000, 0.000000000000000000 ) ) ;
#775 = VECTOR ( 'NONE', #2055, 1000.000000000000000 ) ;
#776 = PRODUCT_DEFINITION ( 'UNKNOWN', '', #1006, #2556 ) ;
#777 = CARTESIAN_POINT ( 'NONE',  ( 9.358389811594321372, -51.26439022220082364, 0.6222967749758763212 ) ) ;
#778 = CARTESIAN_POINT ( 'NONE',  ( -2.250215587473127332, -52.79999999999999716, 8.376503107917878665 ) ) ;
#779 = ORIENTED_EDGE ( 'NONE', *, *, #692, .F. ) ;
#780 = FILL_AREA_STYLE ('',( #1494 ) ) ;
#781 = DIRECTION ( 'NONE',  ( -0.000000000000000000, -0.000000000000000000, 1.000000000000000000 ) ) ;
#782 = DIRECTION ( 'NONE',  ( -0.000000000000000000, -0.000000000000000000, -1.000000000000000000 ) ) ;
#783 = DIRECTION ( 'NONE',  ( -0.000000000000000000, -1.000000000000000000, -0.000000000000000000 ) ) ;
#784 = ORIENTED_EDGE ( 'NONE', *, *, #473, .F. ) ;
#785 = CARTESIAN_POINT ( 'NONE',  ( 4.828119302692784665, -50.75309309120538614, -1.300931117799746906 ) ) ;
#786 = APPLICATION_PROTOCOL_DEFINITION ( 'draft international standard', 'automotive_design', 1998, #1864 ) ;
#787 = CARTESIAN_POINT ( 'NONE',  ( 8.324422814932072257, -47.20000000000001705, 2.231815450537910195 ) ) ;
#788 = DIRECTION ( 'NONE',  ( -0.000000000000000000, -0.000000000000000000, -1.000000000000000000 ) ) ;
#789 = DIRECTION ( 'NONE',  ( -0.000000000000000000, -0.000000000000000000, 1.000000000000000000 ) ) ;
#790 = CARTESIAN_POINT ( 'NONE',  ( 0.000000000000000000, 30.00000000000000000, 18.00000000000000355 ) ) ;
#791 = AXIS2_PLACEMENT_3D ( 'NONE', #2580, #879, #2621 ) ;
#792 = PLANE ( 'NONE',  #1520 ) ;
#793 = CARTESIAN_POINT ( 'NONE',  ( -8.600005876649037262, -50.00000000000000000, -0.2541998246238979520 ) ) ;
#794 = AXIS2_PLACEMENT_3D ( 'NONE', #3254, #1999, #741 ) ;
#795 = ORIENTED_EDGE ( 'NONE', *, *, #2848, .T. ) ;
#796 = FILL_AREA_STYLE_COLOUR ( '', #3038 ) ;
#797 = CARTESIAN_POINT ( 'NONE',  ( -8.572276570256935457, -50.00000000000000000, 0.7042094815226510596 ) ) ;
#798 = CARTESIAN_POINT ( 'NONE',  ( 11.64000000000000057, -50.00000000000000000, 0.000000000000000000 ) ) ;
#799 = ORIENTED_EDGE ( 'NONE', *, *, #2840, .F. ) ;
#800 = CARTESIAN_POINT ( 'NONE',  ( 2.257837506661119154, 7.153666188643283519, -4.464160652961850495 ) ) ;
#801 = CARTESIAN_POINT ( 'NONE',  ( 8.530791689320606608, -47.20000000000001705, 1.124695299888175182 ) ) ;
#802 = ORIENTED_EDGE ( 'NONE', *, *, #1115, .T. ) ;
#803 = CARTESIAN_POINT ( 'NONE',  ( -4.661216347248876346, -73.77919958324079630, 1.816027882404183114 ) ) ;
#804 = EDGE_CURVE ( 'NONE', #694, #2199, #2047, .T. ) ;
#805 = CARTESIAN_POINT ( 'NONE',  ( -1.181079518071022826E-19, -76.00000000000001421, 4.999999999999999112 ) ) ;
#806 = EDGE_LOOP ( 'NONE', ( #2374, #2972, #1302 ) ) ;
#807 = SHAPE_DEFINITION_REPRESENTATION ( #384, #545 ) ;
#808 = DIRECTION ( 'NONE',  ( 1.000000000000000000, 0.000000000000000000, -0.000000000000000000 ) ) ;
#809 = CARTESIAN_POINT ( 'NONE',  ( -8.489369361306263073, -52.79999999999999716, 1.403517616197273554 ) ) ;
#810 = VERTEX_POINT ( 'NONE', #328 ) ;
#811 = EDGE_CURVE ( 'NONE', #335, #2166, #1467, .T. ) ;
#812 = CARTESIAN_POINT ( 'NONE',  ( 0.2675651834338630408, -114.8434534129297191, -0.9733310578110719868 ) ) ;
#813 = CARTESIAN_POINT ( 'NONE',  ( -8.599999999999996092, -50.00000000000000000, -0.5466666666666361030 ) ) ;
#814 = CARTESIAN_POINT ( 'NONE',  ( -5.999999999999992895, -70.00000000000000000, 10.00000000000000000 ) ) ;
#815 = ORIENTED_EDGE ( 'NONE', *, *, #2912, .F. ) ;
#816 = CARTESIAN_POINT ( 'NONE',  ( 0.3369232893658926642, 7.494324649304657804, -4.991499248304590353 ) ) ;
#817 = CARTESIAN_POINT ( 'NONE',  ( -5.285102517542626721, -47.20000000000001705, 6.877134118847253674 ) ) ;
#818 = ORIENTED_EDGE ( 'NONE', *, *, #511, .F. ) ;
#819 = DIRECTION ( 'NONE',  ( 0.000000000000000000, -1.000000000000000000, 0.000000000000000000 ) ) ;
#820 = DIRECTION ( 'NONE',  ( -0.000000000000000000, -1.000000000000000000, -0.000000000000000000 ) ) ;
#821 = VERTEX_POINT ( 'NONE', #863 ) ;
#822 = DIRECTION ( 'NONE',  ( 0.000000000000000000, 0.000000000000000000, 1.000000000000000000 ) ) ;
#823 = CARTESIAN_POINT ( 'NONE',  ( 0.2999999999999837796, -118.9999999999982379, -2.300000000000000266 ) ) ;
#824 = CARTESIAN_POINT ( 'NONE',  ( 6.877134118866901957, -52.79999999999999716, 5.285102517562147995 ) ) ;
#825 = ORIENTED_EDGE ( 'NONE', *, *, #3138, .F. ) ;
#826 = CIRCLE ( 'NONE', #1202, 2.300000000000000266 ) ;
#827 = DIRECTION ( 'NONE',  ( 0.000000000000000000, 0.000000000000000000, -1.000000000000000000 ) ) ;
#828 =( NAMED_UNIT ( * ) PLANE_ANGLE_UNIT ( ) SI_UNIT ( $, .RADIAN. ) );
#829 = CIRCLE ( 'NONE', #2682, 6.000000000000001776 ) ;
#830 = CARTESIAN_POINT ( 'NONE',  ( 8.324422814932070480, -50.00000000000000000, 2.231815450537910639 ) ) ;
#831 = CARTESIAN_POINT ( 'NONE',  ( 2.259265036967212481, -7.158401641891561695, 4.472413388026437175 ) ) ;
#832 = FACE_OUTER_BOUND ( 'NONE', #1836, .T. ) ;
#833 = ORIENTED_EDGE ( 'NONE', *, *, #3154, .T. ) ;
#834 = DIRECTION ( 'NONE',  ( 1.000000000000000000, -0.000000000000000000, -0.000000000000000000 ) ) ;
#835 = ADVANCED_FACE ( 'NONE', ( #1123 ), #1369, .F. ) ;
#836 = AXIS2_PLACEMENT_3D ( 'NONE', #2313, #3274, #2573 ) ;
#837 = EDGE_CURVE ( 'NONE', #2412, #2195, #3144, .T. ) ;
#838 = CARTESIAN_POINT ( 'NONE',  ( -8.600005876649037262, -47.20000000000001705, -0.2541998246238979520 ) ) ;
#839 = ORIENTED_EDGE ( 'NONE', *, *, #1858, .T. ) ;
#840 = CARTESIAN_POINT ( 'NONE',  ( -0.3347605109170348481, -72.48298187229545420, -4.991431073436380039 ) ) ;
#841 = DIRECTION ( 'NONE',  ( -1.000000000000000000, 0.000000000000000000, 0.000000000000000000 ) ) ;
#842 = VERTEX_POINT ( 'NONE', #2836 ) ;
#843 = DIRECTION ( 'NONE',  ( -0.000000000000000000, -0.000000000000000000, 1.000000000000000000 ) ) ;
#844 = CARTESIAN_POINT ( 'NONE',  ( 8.572276570257082895, -52.79999999999999716, 0.7042094815225934390 ) ) ;
#845 = ORIENTED_EDGE ( 'NONE', *, *, #547, .T. ) ;
#846 = VECTOR ( 'NONE', #3111, 1000.000000000000000 ) ;
#847 = CARTESIAN_POINT ( 'NONE',  ( -4.999999999999998224, 30.00000000000000000, 10.00000000000000000 ) ) ;
#848 = FILL_AREA_STYLE_COLOUR ( '', #2121 ) ;
#849 = VECTOR ( 'NONE', #2481, 1000.000000000000000 ) ;
#850 = CARTESIAN_POINT ( 'NONE',  ( -4.769696007084729850, -50.00000000000000000, 1.499999999999994449 ) ) ;
#851 = CARTESIAN_POINT ( 'NONE',  ( 4.477156588595653020, -6.019182485879955635, 2.249288964509364774 ) ) ;
#852 = DIRECTION ( 'NONE',  ( 1.000000000000000000, -0.000000000000000000, -0.000000000000000000 ) ) ;
#853 = ORIENTED_EDGE ( 'NONE', *, *, #1858, .F. ) ;
#854 = DIRECTION ( 'NONE',  ( -0.000000000000000000, 1.000000000000000000, -0.000000000000000000 ) ) ;
#855 = CARTESIAN_POINT ( 'NONE',  ( -11.39999999999999680, -50.00000000000000000, -0.5466666666666361030 ) ) ;
#856 = PRODUCT_DEFINITION_FORMATION_WITH_SPECIFIED_SOURCE ( 'ANY', '', #357, .NOT_KNOWN. ) ;
#857 = EDGE_LOOP ( 'NONE', ( #3078, #2844, #1367, #3, #1429, #1404 ) ) ;
#858 = CARTESIAN_POINT ( 'NONE',  ( 0.000000000000000000, 30.00000000000000000, 10.00000000000000000 ) ) ;
#859 = DIRECTION ( 'NONE',  ( 1.000000000000000000, 0.000000000000000000, 0.000000000000000000 ) ) ;
#860 = ORIENTED_EDGE ( 'NONE', *, *, #3025, .F. ) ;
#861 = CARTESIAN_POINT ( 'NONE',  ( -0.3318670470563950814, -67.51651316714541906, -4.991680947004272006 ) ) ;
#862 = PRODUCT ( 'MAS-169', 'MAS-169', '', ( #1049 ) ) ;
#863 = CARTESIAN_POINT ( 'NONE',  ( -2.499999999999991562, -70.00000000000000000, 10.00000000000000000 ) ) ;
#864 = CARTESIAN_POINT ( 'NONE',  ( 1.269654200241442377, -67.82150855935358891, -4.845952790443002201 ) ) ;
#865 = ORIENTED_EDGE ( 'NONE', *, *, #2062, .F. ) ;
#866 = CYLINDRICAL_SURFACE ( 'NONE', #3223, 6.000000000000001776 ) ;
#867 = CARTESIAN_POINT ( 'NONE',  ( 4.990888858476322021, 5.598354044414833197, 0.3458703032855571791 ) ) ;
#868 = CARTESIAN_POINT ( 'NONE',  ( 11.39999999999999680, -47.20000000000001705, -1.366666666666861873 ) ) ;
#869 = CARTESIAN_POINT ( 'NONE',  ( -11.40000778997679021, -50.00000000000000000, -0.2924664341913127408 ) ) ;
#870 = VERTEX_POINT ( 'NONE', #2333 ) ;
#871 = CARTESIAN_POINT ( 'NONE',  ( -4.823237137747319103, 5.743727463073391881, -1.327965985491348588 ) ) ;
#872 = CARTESIAN_POINT ( 'NONE',  ( 11.30825875096028099, -50.00000000000000000, 1.490875164968454181 ) ) ;
#873 = CARTESIAN_POINT ( 'NONE',  ( 0.2999999999999837796, -114.9999999999982236, -0.9539392014169875145 ) ) ;
#874 = ORIENTED_EDGE ( 'NONE', *, *, #568, .T. ) ;
#875 = CARTESIAN_POINT ( 'NONE',  ( 0.2999999999999963807, -119.0796226588036859, 0.7373253218603739167 ) ) ;
#876 = DIRECTION ( 'NONE',  ( 0.000000000000000000, 0.000000000000000000, -1.000000000000000000 ) ) ;
#877 = CARTESIAN_POINT ( 'NONE',  ( 2.164733944603292493, -68.73913292587020862, -4.508175298354527349 ) ) ;
#878 = ORIENTED_EDGE ( 'NONE', *, *, #2178, .F. ) ;
#879 = DIRECTION ( 'NONE',  ( 0.000000000000000000, -1.000000000000000000, 0.000000000000000000 ) ) ;
#880 =( NAMED_UNIT ( * ) SI_UNIT ( $, .STERADIAN. ) SOLID_ANGLE_UNIT ( ) );
#881 = CARTESIAN_POINT ( 'NONE',  ( -9.116201041289377471, -47.20000000000001705, 7.005833569791151128 ) ) ;
#882 = SURFACE_STYLE_USAGE ( .BOTH. , #2192 ) ;
#883 = CARTESIAN_POINT ( 'NONE',  ( 0.000000000000000000, -84.99999999999998579, 0.000000000000000000 ) ) ;
#884 = CARTESIAN_POINT ( 'NONE',  ( 11.25335008359258282, -47.20000000000001705, 1.860476840074028360 ) ) ;
#885 = ORIENTED_EDGE ( 'NONE', *, *, #2233, .F. ) ;
#886 = PRODUCT_DEFINITION_SHAPE ( 'NONE', 'NONE',  #3057 ) ;
#887 = CARTESIAN_POINT ( 'NONE',  ( 0.000000000000000000, -125.0000000000000000, 1.499999999999999778 ) ) ;
#888 = CONICAL_SURFACE ( 'NONE', #3046, 0.4999999999999813483, 0.04995839572193926104 ) ;
#889 = EDGE_CURVE ( 'NONE', #1696, #890, #2872, .T. ) ;
#890 = VERTEX_POINT ( 'NONE', #2577 ) ;
#891 = DIRECTION ( 'NONE',  ( -0.000000000000000000, -1.000000000000000000, -0.000000000000000000 ) ) ;
#892 = CARTESIAN_POINT ( 'NONE',  ( 0.000000000000000000, 0.000000000000000000, -10.00000000000000000 ) ) ;
#893 = ORIENTED_EDGE ( 'NONE', *, *, #2988, .F. ) ;
#894 = CARTESIAN_POINT ( 'NONE',  ( 0.000000000000000000, -125.0000000000000000, 0.4999999999999813483 ) ) ;
#895 = CARTESIAN_POINT ( 'NONE',  ( 11.39999532361432522, -47.20000000000001705, 0.1755699507458462760 ) ) ;
#896 = CARTESIAN_POINT ( 'NONE',  ( -4.831975997384719612, -5.736714355192817472, -1.328626502536248699 ) ) ;
#897 = DIRECTION ( 'NONE',  ( 0.000000000000000000, 0.000000000000000000, -1.000000000000000000 ) ) ;
#898 = VECTOR ( 'NONE', #3020, 1000.000000000000000 ) ;
#899 = CARTESIAN_POINT ( 'NONE',  ( 11.39539595717860188, -47.20000000000001705, 0.3739757293042009767 ) ) ;
#900 = VERTEX_POINT ( 'NONE', #310 ) ;
#901 =( BOUNDED_SURFACE ( )  B_SPLINE_SURFACE ( 3, 3, ( 
 ( #1734, #2746, #2992, #730, #1989, #2709, #2754, #169, #200, #3201, #1446, #440, #2495, #691, #1944, #2458, #1480, #423, #184, #1744, #707, #1213, #2230, #217, #1229, #1196, #977, #1707, #1980, #1694, #2214, #930, #2983, #3215, #946, #2951, #2196, #963 ),
 ( #2724, #1964, #2691, #2969, #455, #1460, #2477, #231, #3236, #2506, #2245, #1430, #2443, #722, #1243, #1724, #2739, #738, #472, #3251, #489, #2259, #1995, #3001, #1498, #1181, #914, #1927, #2932, #674, #1675, #3166, #622, #2453, #1937, #1176, #2423, #2943 ),
 ( #3183, #2878, #2668, #2407, #1686, #435, #179, #1625, #1407, #2639, #398, #910, #1158, #368, #881, #1668, #1640, #1377, #119, #2913, #1440, #2704, #1423, #685, #1127, #2438, #147, #2191, #1655, #639, #1191, #667, #895, #2176, #131, #3133, #868, #2685 ),
 ( #2654, #1869, #2393, #1392, #653, #2895, #2142, #1921, #3196, #383, #417, #2926, #163, #923, #3149, #1141, #1887, #2158, #1906, #762, #1454, #1492, #1207, #2733, #1719, #496, #1975, #3231, #717, #2760, #1702, #467, #3023, #1990, #2502, #225, #1505, #2516 ),
 ( #2993, #2978, #1472, #2223, #194, #2253, #972, #958, #2487, #3210, #2963, #1224, #702, #210, #3261, #483, #2240, #2719, #241, #2468, #1008, #2205, #1956, #1238, #2006, #733, #991, #939, #1735, #450, #3246, #2747, #1253, #2267, #2, #2023, #3009, #749 ),
 ( #1750, #1765, #513, #2773, #1521, #2529, #258, #3089, #1318, #1019, #809, #549, #3109, #1845, #1603, #3035, #2819, #778, #1813, #2334, #2578, #1780, #2301, #824, #3053, #2787, #1540, #1052, #2858, #844, #2837, #1086, #2548, #581, #566, #329, #3072, #2049 ),
 ( #2036, #2599, #2068, #276, #793, #1335, #2349, #1301, #1798, #13, #2100, #2804, #1568, #1035, #2619, #311, #77, #1555, #1830, #61, #1070, #2085, #1585, #2560, #28, #600, #293, #1268, #531, #2286, #1283, #2317, #44, #1917, #114, #1370, #2139, #906 ) ),
 .UNSPECIFIED., .T., .F., .T. ) 
 B_SPLINE_SURFACE_WITH_KNOTS ( ( 4, 3, 4 ),
 ( 4, 2, 2, 2, 2, 2, 2, 2, 2, 2, 2, 2, 2, 2, 2, 2, 2, 2, 4 ),
 ( 0.000000000000000000, 0.5000000000000000000, 1.000000000000000000 ),
 ( -0.05205660780589810299, -0.02602830390294905150, 0.000000000000000000, 0.01562500000000000000, 0.03125000000000000000, 0.06250000000000000000, 0.1250000000000000000, 0.2500000000000000000, 0.3750000000000000000, 0.5000000000000000000, 0.6250000000000000000, 0.7500000000000000000, 0.8750000000000000000, 0.9375000000000000000, 0.9687500000000000000, 0.9843750000000000000, 1.000000000000000000, 1.026028303902949190, 1.052056607805898381 ),
 .UNSPECIFIED. ) 
 GEOMETRIC_REPRESENTATION_ITEM ( )  RATIONAL_B_SPLINE_SURFACE ( (
 ( 1.000000000000000000, 1.000000000000000000, 1.000000000000000000, 1.000000000000000000, 1.000000000000000000, 1.000000000000000000, 1.000000000000000000, 1.000000000000000000, 1.000000000000000000, 1.000000000000000000, 1.000000000000000000, 1.000000000000000000, 1.000000000000000000, 1.000000000000000000, 1.000000000000000000, 1.000000000000000000, 1.000000000000000000, 1.000000000000000000, 1.000000000000000000, 1.000000000000000000, 1.000000000000000000, 1.000000000000000000, 1.000000000000000000, 1.000000000000000000, 1.000000000000000000, 1.000000000000000000, 1.000000000000000000, 1.000000000000000000, 1.000000000000000000, 1.000000000000000000, 1.000000000000000000, 1.000000000000000000, 1.000000000000000000, 1.000000000000000000, 1.000000000000000000, 1.000000000000000000, 1.000000000000000000, 1.000000000000000000),
 ( 0.3333333333333333703, 0.3333333333333333703, 0.3333333333333333703, 0.3333333333333333703, 0.3333333333333333703, 0.3333333333333333703, 0.3333333333333333703, 0.3333333333333333703, 0.3333333333333333703, 0.3333333333333333703, 0.3333333333333333703, 0.3333333333333333703, 0.3333333333333333703, 0.3333333333333333703, 0.3333333333333333703, 0.3333333333333333703, 0.3333333333333333703, 0.3333333333333333703, 0.3333333333333333703, 0.3333333333333333703, 0.3333333333333333703, 0.3333333333333333703, 0.3333333333333333703, 0.3333333333333333703, 0.3333333333333333703, 0.3333333333333333703, 0.3333333333333333703, 0.3333333333333333703, 0.3333333333333333703, 0.3333333333333333703, 0.3333333333333333703, 0.3333333333333333703, 0.3333333333333333703, 0.3333333333333333703, 0.3333333333333333703, 0.3333333333333333703, 0.3333333333333333703, 0.3333333333333333703),
 ( 0.3333333333333333703, 0.3333333333333333703, 0.3333333333333333703, 0.3333333333333333703, 0.3333333333333333703, 0.3333333333333333703, 0.3333333333333333703, 0.3333333333333333703, 0.3333333333333333703, 0.3333333333333333703, 0.3333333333333333703, 0.3333333333333333703, 0.3333333333333333703, 0.3333333333333333703, 0.3333333333333333703, 0.3333333333333333703, 0.3333333333333333703, 0.3333333333333333703, 0.3333333333333333703, 0.3333333333333333703, 0.3333333333333333703, 0.3333333333333333703, 0.3333333333333333703, 0.3333333333333333703, 0.3333333333333333703, 0.3333333333333333703, 0.3333333333333333703, 0.3333333333333333703, 0.3333333333333333703, 0.3333333333333333703, 0.3333333333333333703, 0.3333333333333333703, 0.3333333333333333703, 0.3333333333333333703, 0.3333333333333333703, 0.3333333333333333703, 0.3333333333333333703, 0.3333333333333333703),
 ( 1.000000000000000000, 1.000000000000000000, 1.000000000000000000, 1.000000000000000000, 1.000000000000000000, 1.000000000000000000, 1.000000000000000000, 1.000000000000000000, 1.000000000000000000, 1.000000000000000000, 1.000000000000000000, 1.000000000000000000, 1.000000000000000000, 1.000000000000000000, 1.000000000000000000, 1.000000000000000000, 1.000000000000000000, 1.000000000000000000, 1.000000000000000000, 1.000000000000000000, 1.000000000000000000, 1.000000000000000000, 1.000000000000000000, 1.000000000000000000, 1.000000000000000000, 1.000000000000000000, 1.000000000000000000, 1.000000000000000000, 1.000000000000000000, 1.000000000000000000, 1.000000000000000000, 1.000000000000000000, 1.000000000000000000, 1.000000000000000000, 1.000000000000000000, 1.000000000000000000, 1.000000000000000000, 1.000000000000000000),
 ( 0.3333333333333333703, 0.3333333333333333703, 0.3333333333333333703, 0.3333333333333333703, 0.3333333333333333703, 0.3333333333333333703, 0.3333333333333333703, 0.3333333333333333703, 0.3333333333333333703, 0.3333333333333333703, 0.3333333333333333703, 0.3333333333333333703, 0.3333333333333333703, 0.3333333333333333703, 0.3333333333333333703, 0.3333333333333333703, 0.3333333333333333703, 0.3333333333333333703, 0.3333333333333333703, 0.3333333333333333703, 0.3333333333333333703, 0.3333333333333333703, 0.3333333333333333703, 0.3333333333333333703, 0.3333333333333333703, 0.3333333333333333703, 0.3333333333333333703, 0.3333333333333333703, 0.3333333333333333703, 0.3333333333333333703, 0.3333333333333333703, 0.3333333333333333703, 0.3333333333333333703, 0.3333333333333333703, 0.3333333333333333703, 0.3333333333333333703, 0.3333333333333333703, 0.3333333333333333703),
 ( 0.3333333333333333703, 0.3333333333333333703, 0.3333333333333333703, 0.3333333333333333703, 0.3333333333333333703, 0.3333333333333333703, 0.3333333333333333703, 0.3333333333333333703, 0.3333333333333333703, 0.3333333333333333703, 0.3333333333333333703, 0.3333333333333333703, 0.3333333333333333703, 0.3333333333333333703, 0.3333333333333333703, 0.3333333333333333703, 0.3333333333333333703, 0.3333333333333333703, 0.3333333333333333703, 0.3333333333333333703, 0.3333333333333333703, 0.3333333333333333703, 0.3333333333333333703, 0.3333333333333333703, 0.3333333333333333703, 0.3333333333333333703, 0.3333333333333333703, 0.3333333333333333703, 0.3333333333333333703, 0.3333333333333333703, 0.3333333333333333703, 0.3333333333333333703, 0.3333333333333333703, 0.3333333333333333703, 0.3333333333333333703, 0.3333333333333333703, 0.3333333333333333703, 0.3333333333333333703),
 ( 1.000000000000000000, 1.000000000000000000, 1.000000000000000000, 1.000000000000000000, 1.000000000000000000, 1.000000000000000000, 1.000000000000000000, 1.000000000000000000, 1.000000000000000000, 1.000000000000000000, 1.000000000000000000, 1.000000000000000000, 1.000000000000000000, 1.000000000000000000, 1.000000000000000000, 1.000000000000000000, 1.000000000000000000, 1.000000000000000000, 1.000000000000000000, 1.000000000000000000, 1.000000000000000000, 1.000000000000000000, 1.000000000000000000, 1.000000000000000000, 1.000000000000000000, 1.000000000000000000, 1.000000000000000000, 1.000000000000000000, 1.000000000000000000, 1.000000000000000000, 1.000000000000000000, 1.000000000000000000, 1.000000000000000000, 1.000000000000000000, 1.000000000000000000, 1.000000000000000000, 1.000000000000000000, 1.000000000000000000) ) ) 
 REPRESENTATION_ITEM ( '' )  SURFACE ( )  );
#902 = CARTESIAN_POINT ( 'NONE',  ( -2.181554758577748387, -71.26329604159570863, -4.501186289107192096 ) ) ;
#903 = VERTEX_POINT ( 'NONE', #2649 ) ;
#904 = CARTESIAN_POINT ( 'NONE',  ( -1.260899024725782080, -67.83519155447288540, -4.840427811610033437 ) ) ;
#905 = DIRECTION ( 'NONE',  ( 1.000000000000000000, 0.000000000000000000, 0.000000000000000000 ) ) ;
#906 = CARTESIAN_POINT ( 'NONE',  ( 8.599999999999996092, -50.00000000000000000, -1.639999999999997460 ) ) ;
#907 = ORIENTED_EDGE ( 'NONE', *, *, #1330, .F. ) ;
#908 = DIRECTION ( 'NONE',  ( 1.000000000000000000, 0.000000000000000000, -0.000000000000000000 ) ) ;
#909 = EDGE_CURVE ( 'NONE', #1621, #1382, #1602, .T. ) ;
#910 = CARTESIAN_POINT ( 'NONE',  ( -11.03470001049236160, -47.20000000000001705, 2.958453039083849045 ) ) ;
#911 = FACE_OUTER_BOUND ( 'NONE', #1807, .T. ) ;
#912 = CARTESIAN_POINT ( 'NONE',  ( -9.116201041288242379, -50.00000000000000000, 7.005833569791151128 ) ) ;
#913 = EDGE_LOOP ( 'NONE', ( #3106, #2620, #845, #2078 ) ) ;
#914 = CARTESIAN_POINT ( 'NONE',  ( 8.324422814932072257, -47.20000000000001705, 2.231815450537910195 ) ) ;
#915 = DIRECTION ( 'NONE',  ( -1.000000000000000000, 0.000000000000000000, 0.000000000000000000 ) ) ;
#916 = DIRECTION ( 'NONE',  ( 1.000000000000000000, 0.000000000000000000, 0.000000000000000000 ) ) ;
#917 = ORIENTED_EDGE ( 'NONE', *, *, #2667, .T. ) ;
#918 = DIRECTION ( 'NONE',  ( 0.000000000000000000, 0.000000000000000000, 1.000000000000000000 ) ) ;
#919 = CARTESIAN_POINT ( 'NONE',  ( 8.530791689320604831, -50.00000000000000000, 1.124695299888175182 ) ) ;
#920 = DIRECTION ( 'NONE',  ( -0.000000000000000000, -0.000000000000000000, -1.000000000000000000 ) ) ;
#921 = CARTESIAN_POINT ( 'NONE',  ( 3.117018002318638459, -75.13542606116712363, 3.922457828541068281 ) ) ;
#922 = FACE_OUTER_BOUND ( 'NONE', #1433, .T. ) ;
#923 = CARTESIAN_POINT ( 'NONE',  ( -9.959683570761574956, -50.00000000000000000, 5.743837162464267898 ) ) ;
#924 = CARTESIAN_POINT ( 'NONE',  ( -4.930411998009738284, -5.651814738127338700, 0.8477781614216437500 ) ) ;
#925 = EDGE_CURVE ( 'NONE', #651, #356, #2618, .T. ) ;
#926 = CARTESIAN_POINT ( 'NONE',  ( -11.29771452881884208, -50.53508261979052918, -1.297714528818841417 ) ) ;
#927 = CARTESIAN_POINT ( 'NONE',  ( 4.331939449206418047, -52.79999999999999716, 7.514224851275111305 ) ) ;
#928 = ORIENTED_EDGE ( 'NONE', *, *, #837, .T. ) ;
#929 = EDGE_CURVE ( 'NONE', #2083, #2713, #1634, .T. ) ;
#930 = CARTESIAN_POINT ( 'NONE',  ( 8.596526774713712626, -50.00000000000000000, 0.2821220414049827596 ) ) ;
#931 = CARTESIAN_POINT ( 'NONE',  ( 6.123233995736765296E-16, -80.00000000000000000, -4.999999999999999112 ) ) ;
#932 = DIRECTION ( 'NONE',  ( 0.000000000000000000, 0.000000000000000000, 1.000000000000000000 ) ) ;
#933 = EDGE_LOOP ( 'NONE', ( #1125, #878, #1413, #2404 ) ) ;
#934 = DIRECTION ( 'NONE',  ( 1.000000000000000000, 0.000000000000000000, 0.000000000000000000 ) ) ;
#935 = CARTESIAN_POINT ( 'NONE',  ( 6.000000000000010658, -70.00000000000000000, 10.00000000000000000 ) ) ;
#936 = DIRECTION ( 'NONE',  ( -0.000000000000000000, -1.000000000000000000, -0.000000000000000000 ) ) ;
#937 = FACE_OUTER_BOUND ( 'NONE', #2646, .T. ) ;
#938 = CARTESIAN_POINT ( 'NONE',  ( -4.828226831489238258, -49.24623717837067716, 1.300528505912509125 ) ) ;
#939 = CARTESIAN_POINT ( 'NONE',  ( 11.25335008359286704, -52.79999999999999716, 1.860476840074311911 ) ) ;
#940 = CARTESIAN_POINT ( 'NONE',  ( 11.39999999999999680, -50.00000000000000000, -0.5466666666666269991 ) ) ;
#941 = CARTESIAN_POINT ( 'NONE',  ( 1.224646799147341621E-16, -125.0000000000000000, -0.4999999999999813483 ) ) ;
#942 = EDGE_CURVE ( 'NONE', #3014, #1569, #378, .T. ) ;
#943 = CARTESIAN_POINT ( 'NONE',  ( -6.877134118866001344, -52.79999999999999716, 5.285102517561345969 ) ) ;
#944 = ORIENTED_EDGE ( 'NONE', *, *, #3118, .T. ) ;
#945 = AXIS2_PLACEMENT_3D ( 'NONE', #2977, #2731, #716 ) ;
#946 = CARTESIAN_POINT ( 'NONE',  ( 8.599999999999996092, -50.00000000000000000, -0.5466666666666269991 ) ) ;
#947 = AXIS2_PLACEMENT_3D ( 'NONE', #632, #1861, #1368 ) ;
#948 = CARTESIAN_POINT ( 'NONE',  ( 11.39999999999999680, -50.00000000000000000, -1.400000000003877254 ) ) ;
#949 = ORIENTED_EDGE ( 'NONE', *, *, #2612, .T. ) ;
#950 = COLOUR_RGB ( '',0.8941176470588234615, 0.8941176470588234615, 0.8941176470588234615 ) ;
#951 = CARTESIAN_POINT ( 'NONE',  ( -5.000000000000000000, 30.00000000000000000, 10.00000000000000178 ) ) ;
#952 = EDGE_CURVE ( 'NONE', #3036, #2217, #1829, .T. ) ;
#953 = DIRECTION ( 'NONE',  ( -1.000000000000000000, 0.000000000000000000, 0.000000000000000000 ) ) ;
#954 = DIRECTION ( 'NONE',  ( 1.000000000000000000, 0.000000000000000000, 0.000000000000000000 ) ) ;
#955 = AXIS2_PLACEMENT_3D ( 'NONE', #309, #822, #2597 ) ;
#956 = CARTESIAN_POINT ( 'NONE',  ( 11.39999999999999680, -50.00000000000000000, -1.400000000003877254 ) ) ;
#957 = CARTESIAN_POINT ( 'NONE',  ( -4.784702204231576772, -49.60930290693747935, -1.451562066005745999 ) ) ;
#958 = CARTESIAN_POINT ( 'NONE',  ( -11.37702123033521850, -52.79999999999999716, 0.7471912688805021352 ) ) ;
#959 = CARTESIAN_POINT ( 'NONE',  ( -0.1572820336012346332, -114.7328664693154963, 1.002697693961912995 ) ) ;
#960 = DIRECTION ( 'NONE',  ( -0.000000000000000000, -0.000000000000000000, 1.000000000000000000 ) ) ;
#961 = CARTESIAN_POINT ( 'NONE',  ( 2.982843918279706408, -52.79999999999999716, 11.10373667793903429 ) ) ;
#962 = ORIENTED_EDGE ( 'NONE', *, *, #1457, .F. ) ;
#963 = CARTESIAN_POINT ( 'NONE',  ( 8.599999999999996092, -50.00000000000000000, -1.639999999999997460 ) ) ;
#964 = CARTESIAN_POINT ( 'NONE',  ( 0.8162268732147681671, -72.36861614780602281, -4.935306302396404554 ) ) ;
#965 = DIRECTION ( 'NONE',  ( -1.000000000000000000, 0.000000000000000000, 0.000000000000000000 ) ) ;
#966 = EDGE_CURVE ( 'NONE', #74, #102, #826, .T. ) ;
#967 = CARTESIAN_POINT ( 'NONE',  ( 6.122861072698252249E-16, -67.50000000000000000, -4.999999999999999112 ) ) ;
#968 = EDGE_CURVE ( 'NONE', #97, #1748, #2385, .T. ) ;
#969 = CARTESIAN_POINT ( 'NONE',  ( -11.39999999999999680, -47.20000000000001705, -1.093333333333363022 ) ) ;
#970 = LINE ( 'NONE', #1953, #1479 ) ;
#971 = CARTESIAN_POINT ( 'NONE',  ( 4.476097271599868144, -74.00023062533671236, 2.250477508087392220 ) ) ;
#972 = CARTESIAN_POINT ( 'NONE',  ( -11.39539595717873510, -52.79999999999999716, 0.3739757293043587949 ) ) ;
#973 = CARTESIAN_POINT ( 'NONE',  ( 11.36325033731732503, -50.00000000000000000, 0.9334869871343942638 ) ) ;
#974 = CARTESIAN_POINT ( 'NONE',  ( -9.597428871122712479, -51.34559595270263799, 0.3947853969006087649 ) ) ;
#975 = CARTESIAN_POINT ( 'NONE',  ( -8.599999999999996092, -50.00000000000000000, -1.366666666666159768 ) ) ;
#976 = ORIENTED_EDGE ( 'NONE', *, *, #3240, .T. ) ;
#977 = CARTESIAN_POINT ( 'NONE',  ( 8.324422814932070480, -50.00000000000000000, 2.231815450537910639 ) ) ;
#978 = ADVANCED_FACE ( 'NONE', ( #3108 ), #2402, .T. ) ;
#979 = CARTESIAN_POINT ( 'NONE',  ( 4.823237137747319103, -5.743727463073391881, -1.327965985491348588 ) ) ;
#980 = VECTOR ( 'NONE', #3128, 1000.000000000000000 ) ;
#981 = LINE ( 'NONE', #2447, #849 ) ;
#982=STYLED_ITEM('',(#3300),#1595);
#983 = EDGE_CURVE ( 'NONE', #1926, #1036, #1773, .T. ) ;
#984 = CARTESIAN_POINT ( 'NONE',  ( 8.599999999999996092, -47.20000000000001705, -0.5466666666666269991 ) ) ;
#985 = CARTESIAN_POINT ( 'NONE',  ( 5.000000000000000000, 30.00000000000000000, 10.00000000000000178 ) ) ;
#986 = EDGE_CURVE ( 'NONE', #335, #3146, #1698, .T. ) ;
#987 = CARTESIAN_POINT ( 'NONE',  ( 11.20659079646779510, -50.71729705017420997, -1.206590796467808646 ) ) ;
#988 = VECTOR ( 'NONE', #1809, 1000.000000000000000 ) ;
#989 = DIRECTION ( 'NONE',  ( -1.000000000000000000, 0.000000000000000000, -0.000000000000000000 ) ) ;
#990 = AXIS2_PLACEMENT_3D ( 'NONE', #359, #2115, #325 ) ;
#991 = CARTESIAN_POINT ( 'NONE',  ( 11.03470001049091032, -52.79999999999999716, 2.958453039085699565 ) ) ;
#992 = CARTESIAN_POINT ( 'NONE',  ( 11.39999532361432522, -50.00000000000000000, 0.1755699507458462760 ) ) ;
#993 = CARTESIAN_POINT ( 'NONE',  ( 0.2999999999999837796, -114.9999999999982236, -0.9539392014169875145 ) ) ;
#994 = CARTESIAN_POINT ( 'NONE',  ( -1.492255338562904265, -52.79999999999999716, 11.39999999999999680 ) ) ;
#995 = EDGE_CURVE ( 'NONE', #821, #123, #1461, .T. ) ;
#996 = ORIENTED_EDGE ( 'NONE', *, *, #1967, .T. ) ;
#997 = CARTESIAN_POINT ( 'NONE',  ( -7.500000000000000000, 0.000000000000000000, 18.00000000000000355 ) ) ;
#998 = CARTESIAN_POINT ( 'NONE',  ( -1.698458751326834992, -64.23621591387086482, 4.714595771049563844 ) ) ;
#999 = CIRCLE ( 'NONE', #2057, 2.500000000000000000 ) ;
#1000 = LINE ( 'NONE', #541, #1002 ) ;
#1001 = PRODUCT_DEFINITION_CONTEXT ( 'detailed design', #2486, 'design' ) ;
#1002 = VECTOR ( 'NONE', #758, 1000.000000000000000 ) ;
#1003 = CARTESIAN_POINT ( 'NONE',  ( 11.64000000000000057, -50.00000000000000000, 1.399999999999999911 ) ) ;
#1004 = LINE ( 'NONE', #11, #2832 ) ;
#1005 = VECTOR ( 'NONE', #3187, 1000.000000000000000 ) ;
#1006 = PRODUCT_DEFINITION_FORMATION_WITH_SPECIFIED_SOURCE ( 'ANY', '', #1626, .NOT_KNOWN. ) ;
#1007 = PLANE ( 'NONE',  #1150 ) ;
#1008 = CARTESIAN_POINT ( 'NONE',  ( 2.982843918279706408, -52.79999999999999716, 11.10373667793903429 ) ) ;
#1009 = ORIENTED_EDGE ( 'NONE', *, *, #2612, .F. ) ;
#1010 = CARTESIAN_POINT ( 'NONE',  ( 0.1572820336012347164, -114.7328664693154678, -1.002697693961912995 ) ) ;
#1011 = CARTESIAN_POINT ( 'NONE',  ( 4.331939449206418935, -50.00000000000000000, 7.514224851275112194 ) ) ;
#1012 = ORIENTED_EDGE ( 'NONE', *, *, #2852, .T. ) ;
#1013 = CARTESIAN_POINT ( 'NONE',  ( 4.916102558146631551, -51.19836246274143576, -0.9228986618089604077 ) ) ;
#1014 = CARTESIAN_POINT ( 'NONE',  ( -4.999999999999999112, -66.68337520964460907, 0.000000000000000000 ) ) ;
#1015 = CARTESIAN_POINT ( 'NONE',  ( -2.592701047953011706, -75.41913213518454029, 4.287209529367745908 ) ) ;
#1016 = CARTESIAN_POINT ( 'NONE',  ( -5.000000000000000000, 5.590169943749474513, 18.00000000000000355 ) ) ;
#1017 = CYLINDRICAL_SURFACE ( 'NONE', #2572, 2.500000000000000444 ) ;
#1018 = DIRECTION ( 'NONE',  ( 0.000000000000000000, -1.000000000000000000, 0.000000000000000000 ) ) ;
#1019 = CARTESIAN_POINT ( 'NONE',  ( -8.530791689320901483, -52.79999999999999716, 1.124695299888049504 ) ) ;
#1020 = ORIENTED_EDGE ( 'NONE', *, *, #98, .T. ) ;
#1021 = CARTESIAN_POINT ( 'NONE',  ( 0.000000000000000000, -80.00000000000000000, -2.500000000000000444 ) ) ;
#1022 = CARTESIAN_POINT ( 'NONE',  ( -5.000000000000000000, 5.590169943749473624, 18.00000000000000355 ) ) ;
#1023 = ADVANCED_FACE ( 'NONE', ( #713, #1933 ), #3224, .T. ) ;
#1024 = FACE_OUTER_BOUND ( 'NONE', #3097, .T. ) ;
#1025 = DIRECTION ( 'NONE',  ( -0.000000000000000000, -0.000000000000000000, 1.000000000000000000 ) ) ;
#1026 = B_SPLINE_CURVE_WITH_KNOTS ( 'NONE', 3,
 ( #110, #3105, #2594, #2345, #2614, #2381 ),
 .UNSPECIFIED., .F., .F.,
 ( 4, 2, 4 ),
 ( 1.973209580890601712E-07, 0.0002370058433632465738, 0.0004738143657684039823 ),
 .UNSPECIFIED. ) ;
#1027 = ORIENTED_EDGE ( 'NONE', *, *, #1712, .F. ) ;
#1028 = CARTESIAN_POINT ( 'NONE',  ( 4.772823865982902092, -50.19777939995103111, -1.490154340647099174 ) ) ;
#1029 = EDGE_CURVE ( 'NONE', #721, #3070, #239, .T. ) ;
#1030 = FACE_OUTER_BOUND ( 'NONE', #1593, .T. ) ;
#1031 = CARTESIAN_POINT ( 'NONE',  ( 0.000000000000000000, 30.00000000000000000, 18.00000000000000355 ) ) ;
#1032 = CARTESIAN_POINT ( 'NONE',  ( 5.000000000000000000, 30.00000000000000000, 18.00000000000000355 ) ) ;
#1033 = CARTESIAN_POINT ( 'NONE',  ( 0.000000000000000000, 0.000000000000000000, 0.000000000000000000 ) ) ;
#1034 = DIRECTION ( 'NONE',  ( 1.000000000000000000, -0.000000000000000000, -0.000000000000000000 ) ) ;
#1035 = CARTESIAN_POINT ( 'NONE',  ( -7.513445500749800665, -50.00000000000000000, 4.333070140105378165 ) ) ;
#1036 = VERTEX_POINT ( 'NONE', #158 ) ;
#1037 = AXIS2_PLACEMENT_3D ( 'NONE', #2701, #2003, #2434 ) ;
#1038 = VECTOR ( 'NONE', #27, 1000.000000000000000 ) ;
#1039 = CARTESIAN_POINT ( 'NONE',  ( 8.596526774713712626, -50.00000000000000000, 0.2821220414049827596 ) ) ;
#1040 = CARTESIAN_POINT ( 'NONE',  ( -3.767802750538409295, -6.489812437959999514, 3.302060000734929446 ) ) ;
#1041 = ORIENTED_EDGE ( 'NONE', *, *, #968, .T. ) ;
#1042 = CARTESIAN_POINT ( 'NONE',  ( 4.871117609892888112, -50.99113739012668844, 1.130144156083558560 ) ) ;
#1043 = EDGE_CURVE ( 'NONE', #3266, #2549, #1186, .T. ) ;
#1044 = APPLICATION_PROTOCOL_DEFINITION ( 'draft international standard', 'automotive_design', 1998, #391 ) ;
#1045 = CARTESIAN_POINT ( 'NONE',  ( 8.599999999999996092, -47.20000000000001705, -1.366666666666861873 ) ) ;
#1046 = VERTEX_POINT ( 'NONE', #1951 ) ;
#1047 = CARTESIAN_POINT ( 'NONE',  ( -4.325729160396026174, -74.16467322009297902, 2.526449232236037901 ) ) ;
#1048 = CARTESIAN_POINT ( 'NONE',  ( -3.854351720261343002E-15, -119.2999999999982776, -0.7850000000000663114 ) ) ;
#1049 = PRODUCT_CONTEXT ( 'NONE', #1345, 'mechanical' ) ;
#1050 = ADVANCED_FACE ( 'NONE', ( #2201 ), #9, .T. ) ;
#1051 = DIRECTION ( 'NONE',  ( 1.000000000000000000, 0.000000000000000000, 0.000000000000000000 ) ) ;
#1052 = CARTESIAN_POINT ( 'NONE',  ( 8.489369361306732031, -52.79999999999999716, 1.403517616196621409 ) ) ;
#1053 = AXIS2_PLACEMENT_3D ( 'NONE', #1447, #1968, #2711 ) ;
#1054 = VERTEX_POINT ( 'NONE', #264 ) ;
#1055 = CARTESIAN_POINT ( 'NONE',  ( 0.000000000000000000, 0.000000000000000000, 10.00000000000000000 ) ) ;
#1056 = PRODUCT_RELATED_PRODUCT_CATEGORY ( 'part', '', ( #1626 ) ) ;
#1057 =( NAMED_UNIT ( * ) SI_UNIT ( $, .STERADIAN. ) SOLID_ANGLE_UNIT ( ) );
#1058 = AXIS2_PLACEMENT_3D ( 'NONE', #3140, #2850, #1876 ) ;
#1059 = CARTESIAN_POINT ( 'NONE',  ( 0.000000000000000000, -80.00000000000000000, 4.999999999999999112 ) ) ;
#1060 = CARTESIAN_POINT ( 'NONE',  ( 0.000000000000000000, 0.000000000000000000, 10.00000000000000000 ) ) ;
#1061 = ORIENTED_EDGE ( 'NONE', *, *, #1712, .T. ) ;
#1062 = CARTESIAN_POINT ( 'NONE',  ( 0.1685493663350521309, 7.499999999999996447, -4.999999999999998224 ) ) ;
#1063 = APPLICATION_PROTOCOL_DEFINITION ( 'draft international standard', 'automotive_design', 1998, #2986 ) ;
#1064 = CARTESIAN_POINT ( 'NONE',  ( 9.116201041286979390, -47.20000000000001705, 7.005833569791843907 ) ) ;
#1065 = EDGE_LOOP ( 'NONE', ( #1169, #1973 ) ) ;
#1066 = CARTESIAN_POINT ( 'NONE',  ( -4.784761898981735762, -50.39152470491934821, 1.451366868840367808 ) ) ;
#1067 = LINE ( 'NONE', #1032, #245 ) ;
#1068 = EDGE_LOOP ( 'NONE', ( #779, #2813, #3041 ) ) ;
#1069 = DIRECTION ( 'NONE',  ( 0.000000000000000000, 1.000000000000000000, 0.000000000000000000 ) ) ;
#1070 = CARTESIAN_POINT ( 'NONE',  ( 2.250215587473118450, -50.00000000000000000, 8.376503107919017310 ) ) ;
#1071 = ORIENTED_EDGE ( 'NONE', *, *, #3122, .T. ) ;
#1072 = DIRECTION ( 'NONE',  ( 1.000000000000000000, 0.000000000000000000, 0.000000000000000000 ) ) ;
#1073 = DIRECTION ( 'NONE',  ( 1.000000000000000000, 0.000000000000000000, 0.000000000000000000 ) ) ;
#1074 = CARTESIAN_POINT ( 'NONE',  ( 4.863431995609888148, -5.709553999929329215, 1.172553935287278248 ) ) ;
#1075 = CARTESIAN_POINT ( 'NONE',  ( -2.543133226181223616, -7.061565991568797607, 4.317068135836759524 ) ) ;
#1076 = EDGE_LOOP ( 'NONE', ( #1151, #2229, #414, #1587, #3090 ) ) ;
#1077 = CARTESIAN_POINT ( 'NONE',  ( -0.3416648584763157803, 7.500000000000000888, 5.000000000000000888 ) ) ;
#1078 = CARTESIAN_POINT ( 'NONE',  ( 1.125736483477000061, -47.20000000000001705, 8.599999999999996092 ) ) ;
#1079 = ORIENTED_EDGE ( 'NONE', *, *, #3194, .T. ) ;
#1080 = DIRECTION ( 'NONE',  ( 0.000000000000000000, -1.000000000000000000, 0.000000000000000000 ) ) ;
#1081 = CARTESIAN_POINT ( 'NONE',  ( -8.452889752740315288, -50.00000000000000711, 1.586704117746376097 ) ) ;
#1082 = EDGE_LOOP ( 'NONE', ( #2838, #2584, #3073, #1400, #294, #1363, #1309, #1742, #3103, #2595, #2676, #706 ) ) ;
#1083 =( LENGTH_UNIT ( ) NAMED_UNIT ( * ) SI_UNIT ( .MILLI., .METRE. ) );
#1084 = EDGE_CURVE ( 'NONE', #3146, #3014, #510, .T. ) ;
#1085 = CARTESIAN_POINT ( 'NONE',  ( 2.500000000000004441, -71.46446609406727646, 1.464466094067262025 ) ) ;
#1086 = CARTESIAN_POINT ( 'NONE',  ( 8.596526774713710850, -52.79999999999999716, 0.2821220414049827041 ) ) ;
#1087 = VERTEX_POINT ( 'NONE', #2290 ) ;
#1088 = AXIS2_PLACEMENT_3D ( 'NONE', #1909, #3098, #2409 ) ;
#1089 = CARTESIAN_POINT ( 'NONE',  ( 0.000000000000000000, -104.9999999999982379, 1.499999999999999778 ) ) ;
#1090 = CARTESIAN_POINT ( 'NONE',  ( 4.831975997384719612, 5.736714355192817472, -1.328626502536248699 ) ) ;
#1091 = CARTESIAN_POINT ( 'NONE',  ( 4.722607672194940598, -5.826754641390677669, 1.650547109183062355 ) ) ;
#1092 = CARTESIAN_POINT ( 'NONE',  ( 8.324422814932070480, -50.00000000000000000, 2.231815450537910639 ) ) ;
#1093 = VERTEX_POINT ( 'NONE', #1059 ) ;
#1094 = CARTESIAN_POINT ( 'NONE',  ( -1.336826802926396995, 7.387368010283515751, -4.829679162932221992 ) ) ;
#1095 = AXIS2_PLACEMENT_3D ( 'NONE', #2630, #1582, #841 ) ;
#1096 = B_SPLINE_CURVE_WITH_KNOTS ( 'NONE', 3,
 ( #1403, #1124, #1882, #2635 ),
 .UNSPECIFIED., .F., .F.,
 ( 4, 4 ),
 ( 0.005006932180914174663, 0.009012567534305281416 ),
 .UNSPECIFIED. ) ;
#1097 = CARTESIAN_POINT ( 'NONE',  ( 9.116201041287551377, -50.00000000000000000, 7.005833569791843018 ) ) ;
#1098 = AXIS2_PLACEMENT_3D ( 'NONE', #2889, #2386, #113 ) ;
#1099 = CARTESIAN_POINT ( 'NONE',  ( -8.485280282859319456, -49.76857949351400379, 1.400000000000003020 ) ) ;
#1100 = CARTESIAN_POINT ( 'NONE',  ( -1.125736483476999839, -50.00000000000000000, 8.599999999999996092 ) ) ;
#1101 = ORIENTED_EDGE ( 'NONE', *, *, #3177, .F. ) ;
#1102 = FACE_OUTER_BOUND ( 'NONE', #1614, .T. ) ;
#1103 = CARTESIAN_POINT ( 'NONE',  ( 8.485280282859411827, -49.76857949351400379, 1.400000000000001243 ) ) ;
#1104 = ORIENTED_EDGE ( 'NONE', *, *, #2999, .F. ) ;
#1105 = VECTOR ( 'NONE', #146, 1000.000000000000000 ) ;
#1106 = CARTESIAN_POINT ( 'NONE',  ( 0.2999999999999837796, -117.6667267801783225, 0.8135312584238993949 ) ) ;
#1107 =( LENGTH_UNIT ( ) NAMED_UNIT ( * ) SI_UNIT ( .MILLI., .METRE. ) );
#1108 = CIRCLE ( 'NONE', #2274, 7.500000000000000000 ) ;
#1109 = CARTESIAN_POINT ( 'NONE',  ( 4.930411998009738284, 5.651814738127338700, 0.8477781614216437500 ) ) ;
#1110 = CARTESIAN_POINT ( 'NONE',  ( 2.500000000000008438, -70.00000000000000000, 10.00000000000000000 ) ) ;
#1111 = CARTESIAN_POINT ( 'NONE',  ( -3.320792018548207825, -6.729571896343306214, -3.751470290485135806 ) ) ;
#1112 = ORIENTED_EDGE ( 'NONE', *, *, #433, .T. ) ;
#1113 = PRESENTATION_LAYER_ASSIGNMENT (  '', '', ( #590 ) ) ;
#1114 = CARTESIAN_POINT ( 'NONE',  ( -4.725421832813011314, 5.824466512821798503, -1.642406358834817004 ) ) ;
#1115 = EDGE_CURVE ( 'NONE', #2713, #1541, #2925, .T. ) ;
#1116 = CARTESIAN_POINT ( 'NONE',  ( -11.39539595717873510, -52.79999999999999716, 0.3739757293043587949 ) ) ;
#1117 = AXIS2_PLACEMENT_3D ( 'NONE', #774, #2576, #546 ) ;
#1118 = EDGE_CURVE ( 'NONE', #1349, #2923, #2828, .T. ) ;
#1119 = DIRECTION ( 'NONE',  ( -0.000000000000000000, 1.000000000000000000, -0.000000000000000000 ) ) ;
#1120 = CYLINDRICAL_SURFACE ( 'NONE', #2368, 4.999999999999999112 ) ;
#1121 = EDGE_LOOP ( 'NONE', ( #833, #2302 ) ) ;
#1122 = CARTESIAN_POINT ( 'NONE',  ( 2.500000000000000000, 0.000000000000000000, 18.00000000000000355 ) ) ;
#1123 = FACE_OUTER_BOUND ( 'NONE', #3181, .T. ) ;
#1124 = CARTESIAN_POINT ( 'NONE',  ( -0.3000000000000161982, -116.3333805752222929, 0.8840510694876354547 ) ) ;
#1125 = ORIENTED_EDGE ( 'NONE', *, *, #464, .F. ) ;
#1126 = CARTESIAN_POINT ( 'NONE',  ( 0.2999999999999999889, -114.9999999999982236, 0.9539392014169838507 ) ) ;
#1127 = CARTESIAN_POINT ( 'NONE',  ( 9.959683570760009985, -47.20000000000001705, 5.743837162466679302 ) ) ;
#1128 =( REPRESENTATION_RELATIONSHIP ('NONE','NONE', #545, #3271 ) REPRESENTATION_RELATIONSHIP_WITH_TRANSFORMATION ( #1277 )SHAPE_REPRESENTATION_RELATIONSHIP( ) );
#1129 = CARTESIAN_POINT ( 'NONE',  ( 6.124525076959063726E-16, 7.500000000000000000, -4.999999999999999112 ) ) ;
#1130 = ADVANCED_FACE ( 'NONE', ( #1524 ), #2535, .T. ) ;
#1131 = CARTESIAN_POINT ( 'NONE',  ( -2.982843918280285944, -50.00000000000000000, 11.10373667793902541 ) ) ;
#1132 = VERTEX_POINT ( 'NONE', #18 ) ;
#1133 = CYLINDRICAL_SURFACE ( 'NONE', #1058, 1.399999999999999911 ) ;
#1134 = ADVANCED_FACE ( 'NONE', ( #1024 ), #3039, .F. ) ;
#1135 = EDGE_LOOP ( 'NONE', ( #2875, #151, #2955, #2834 ) ) ;
#1136 = CARTESIAN_POINT ( 'NONE',  ( -2.483052435257200319, -69.66568987240576405, -4.340030773391345242 ) ) ;
#1137 = DIRECTION ( 'NONE',  ( 1.000000000000000000, 0.000000000000000000, 0.000000000000000000 ) ) ;
#1138 = CARTESIAN_POINT ( 'NONE',  ( 9.595856219367004059, -48.65479562300421890, 0.3963015081148715257 ) ) ;
#1139 = VERTEX_POINT ( 'NONE', #281 ) ;
#1140 = CARTESIAN_POINT ( 'NONE',  ( 0.000000000000000000, -84.99999999999998579, 2.300000000000000266 ) ) ;
#1141 = CARTESIAN_POINT ( 'NONE',  ( -7.005833569765055557, -50.00000000000000000, 9.116201041262108618 ) ) ;
#1142 = CARTESIAN_POINT ( 'NONE',  ( -4.956114419722681852, -5.629162412197389109, 0.6822959203856070465 ) ) ;
#1143 = CARTESIAN_POINT ( 'NONE',  ( -4.863431995609888148, 5.709553999929329215, 1.172553935287278248 ) ) ;
#1144 = AXIS2_PLACEMENT_3D ( 'NONE', #1475, #960, #1977 ) ;
#1145 = CARTESIAN_POINT ( 'NONE',  ( -9.959683570761574956, -52.79999999999999716, 5.743837162464267898 ) ) ;
#1146 = VERTEX_POINT ( 'NONE', #850 ) ;
#1147 = EDGE_CURVE ( 'NONE', #97, #1979, #1624, .T. ) ;
#1148 = PRODUCT_DEFINITION_SHAPE ( 'NONE', 'NONE',  #3279 ) ;
#1149 = CARTESIAN_POINT ( 'NONE',  ( -5.000000000000001776, -73.31662479035541935, 0.1770536369485815331 ) ) ;
#1150 = AXIS2_PLACEMENT_3D ( 'NONE', #761, #1764, #748 ) ;
#1151 = ORIENTED_EDGE ( 'NONE', *, *, #1928, .F. ) ;
#1152 = SURFACE_SIDE_STYLE ('',( #1618 ) ) ;
#1153 = EDGE_CURVE ( 'NONE', #1895, #84, #746, .T. ) ;
#1154 = CARTESIAN_POINT ( 'NONE',  ( -8.600005876649037262, -50.00000000000000000, -0.2541998246238979520 ) ) ;
#1155 = CARTESIAN_POINT ( 'NONE',  ( 0.000000000000000000, -60.00000000000000000, -2.500000000000000444 ) ) ;
#1156 = VERTEX_POINT ( 'NONE', #2322 ) ;
#1157 = PLANE ( 'NONE',  #2586 ) ;
#1158 = CARTESIAN_POINT ( 'NONE',  ( -10.81682914263834405, -47.20000000000001705, 3.675996170188739143 ) ) ;
#1159 = AXIS2_PLACEMENT_3D ( 'NONE', #650, #2663, #143 ) ;
#1160 = SURFACE_STYLE_FILL_AREA ( #1907 ) ;
#1161 = CARTESIAN_POINT ( 'NONE',  ( -3.854351720261343002E-15, -119.2999999999982776, -0.7850000000000663114 ) ) ;
#1162 = AXIS2_PLACEMENT_3D ( 'NONE', #768, #2279, #2755 ) ;
#1163 = CARTESIAN_POINT ( 'NONE',  ( -7.005833569765055557, -50.00000000000000000, 9.116201041262108618 ) ) ;
#1164 =( GEOMETRIC_REPRESENTATION_CONTEXT ( 3 ) GLOBAL_UNCERTAINTY_ASSIGNED_CONTEXT ( ( #1792 ) ) GLOBAL_UNIT_ASSIGNED_CONTEXT ( ( #1945, #2710, #3216 ) ) REPRESENTATION_CONTEXT ( 'NONE', 'WORKASPACE' ) );
#1165 = ORIENTED_EDGE ( 'NONE', *, *, #942, .F. ) ;
#1166 = ADVANCED_FACE ( 'NONE', ( #3028 ), #2553, .T. ) ;
#1167 = CARTESIAN_POINT ( 'NONE',  ( 2.417876621355959710, -70.65655750441386829, -4.376674006154569696 ) ) ;
#1168 = CARTESIAN_POINT ( 'NONE',  ( 6.121942914840092871E-16, -7.500000000000000000, -4.999999999999999112 ) ) ;
#1169 = ORIENTED_EDGE ( 'NONE', *, *, #1285, .T. ) ;
#1170 = FACE_OUTER_BOUND ( 'NONE', #1076, .T. ) ;
#1171 = CARTESIAN_POINT ( 'NONE',  ( 8.599999999999996092, -50.00000000000000000, -1.639999999999997460 ) ) ;
#1172 = CARTESIAN_POINT ( 'NONE',  ( 2.243056629538943803, -68.88414527589007719, -4.469195550069930967 ) ) ;
#1173 = CARTESIAN_POINT ( 'NONE',  ( 3.984264206898686211, -74.49240233626514396, 3.036427941355731797 ) ) ;
#1174 = CARTESIAN_POINT ( 'NONE',  ( -4.985720285031673527, -48.54819230487149895, -0.3898302721915644087 ) ) ;
#1175 = EDGE_CURVE ( 'NONE', #2825, #1564, #522, .T. ) ;
#1176 = CARTESIAN_POINT ( 'NONE',  ( 8.599999999999996092, -47.20000000000001705, -1.093333333333372126 ) ) ;
#1177 = CARTESIAN_POINT ( 'NONE',  ( 3.061616997868384127E-16, -67.50000000000000000, 2.500000000000000444 ) ) ;
#1178 = CARTESIAN_POINT ( 'NONE',  ( 0.2999999999999999334, -119.0797001093845893, -0.7373211444866922815 ) ) ;
#1179 = CARTESIAN_POINT ( 'NONE',  ( 9.959683570761143301, -52.79999999999999716, 5.743837162466679302 ) ) ;
#1180 = ORIENTED_EDGE ( 'NONE', *, *, #837, .F. ) ;
#1181 = CARTESIAN_POINT ( 'NONE',  ( 8.160064090060387798, -47.20000000000001705, 2.773119917860402239 ) ) ;
#1182 = DIRECTION ( 'NONE',  ( 0.000000000000000000, 1.000000000000000000, 0.000000000000000000 ) ) ;
#1183 = CARTESIAN_POINT ( 'NONE',  ( 11.33515354614431025, -49.56496474501408755, -1.335153546144312919 ) ) ;
#1184 = ORIENTED_EDGE ( 'NONE', *, *, #234, .T. ) ;
#1185 = CARTESIAN_POINT ( 'NONE',  ( 2.592701047953016147, -64.58086786481547392, 4.287209529367743244 ) ) ;
#1186 = LINE ( 'NONE', #2715, #1939 ) ;
#1187 = CARTESIAN_POINT ( 'NONE',  ( 1.464466094067263358, -67.50000000000000000, -2.500000000000002220 ) ) ;
#1188 = CARTESIAN_POINT ( 'NONE',  ( 0.3480864936855372904, -75.99245047245101148, 4.990948402655850380 ) ) ;
#1189 = EDGE_CURVE ( 'NONE', #2794, #1839, #2601, .T. ) ;
#1190 = CARTESIAN_POINT ( 'NONE',  ( -4.815134987083422580, -49.33398324077673180, 1.347591700989805741 ) ) ;
#1191 = CARTESIAN_POINT ( 'NONE',  ( 11.37702123033534995, -47.20000000000001705, 0.7471912688806705560 ) ) ;
#1192 = CARTESIAN_POINT ( 'NONE',  ( 4.815279722017292485, -49.33289952491914931, -1.347079874192880444 ) ) ;
#1193 = DIRECTION ( 'NONE',  ( 0.000000000000000000, 0.000000000000000000, -1.000000000000000000 ) ) ;
#1194 = CARTESIAN_POINT ( 'NONE',  ( 1.492255338562904265, -52.79999999999999716, 11.39999999999999680 ) ) ;
#1195 = VERTEX_POINT ( 'NONE', #557 ) ;
#1196 = CARTESIAN_POINT ( 'NONE',  ( 8.160064090060387798, -50.00000000000000000, 2.773119917860402239 ) ) ;
#1197 =( GEOMETRIC_REPRESENTATION_CONTEXT ( 3 ) GLOBAL_UNCERTAINTY_ASSIGNED_CONTEXT ( ( #3048 ) ) GLOBAL_UNIT_ASSIGNED_CONTEXT ( ( #30, #278, #3056 ) ) REPRESENTATION_CONTEXT ( 'NONE', 'WORKASPACE' ) );
#1198 = LINE ( 'NONE', #931, #2596 ) ;
#1199 = DIRECTION ( 'NONE',  ( 1.000000000000000000, 0.000000000000000000, 0.000000000000000000 ) ) ;
#1200 = ORIENTED_EDGE ( 'NONE', *, *, #2712, .F. ) ;
#1201 = CARTESIAN_POINT ( 'NONE',  ( 3.117741096646119203, -64.86494573768398197, 3.921983519476098135 ) ) ;
#1202 = AXIS2_PLACEMENT_3D ( 'NONE', #3088, #580, #1351 ) ;
#1203 = DIRECTION ( 'NONE',  ( 0.000000000000000000, 1.000000000000000000, 0.000000000000000000 ) ) ;
#1204 = CARTESIAN_POINT ( 'NONE',  ( 0.000000000000000000, -104.9999999999982379, 0.000000000000000000 ) ) ;
#1205 = CARTESIAN_POINT ( 'NONE',  ( 11.38628138490143016, -50.22360298513552124, -1.386281384901437264 ) ) ;
#1206 = CARTESIAN_POINT ( 'NONE',  ( 7.500000000000000888, 30.00000000000000000, 18.00000000000000355 ) ) ;
#1207 = CARTESIAN_POINT ( 'NONE',  ( 7.005833569765714586, -50.00000000000000000, 9.116201041261451365 ) ) ;
#1208 = CARTESIAN_POINT ( 'NONE',  ( 0.000000000000000000, 0.000000000000000000, 10.00000000000000000 ) ) ;
#1209 = CYLINDRICAL_SURFACE ( 'NONE', #86, 4.999999999999999112 ) ;
#1210 = CARTESIAN_POINT ( 'NONE',  ( 8.599999999999996092, -52.79999999999999716, -0.5466666666666269991 ) ) ;
#1211 = ORIENTED_EDGE ( 'NONE', *, *, #411, .T. ) ;
#1212 = AXIS2_PLACEMENT_3D ( 'NONE', #1488, #1986, #1731 ) ;
#1213 = CARTESIAN_POINT ( 'NONE',  ( 4.331939449206418935, -50.00000000000000000, 7.514224851275112194 ) ) ;
#1214 = DIRECTION ( 'NONE',  ( 0.000000000000000000, 0.000000000000000000, -1.000000000000000000 ) ) ;
#1215 = VECTOR ( 'NONE', #788, 1000.000000000000000 ) ;
#1216 = CYLINDRICAL_SURFACE ( 'NONE', #2435, 2.499999999999999556 ) ;
#1217 = B_SPLINE_CURVE_WITH_KNOTS ( 'NONE', 3,
 ( #284, #21, #1560, #3042, #2826, #2566, #1042, #574, #754, #301, #1509, #1310, #4, #268, #1258, #319, #51, #1327, #1013, #34, #2043, #785, #2028, #249, #2293, #1028, #1787, #2796 ),
 .UNSPECIFIED., .F., .F.,
 ( 4, 2, 2, 2, 2, 2, 2, 2, 2, 2, 2, 2, 2, 4 ),
 ( 0.004716923349278730540, 0.005306377133062306975, 0.005601104024954096060, 0.005895830916845884277, 0.006485284700629445967, 0.006780011592521222909, 0.007074738484412999850, 0.007369465376304777660, 0.007664192268196553734, 0.008253646051980109352, 0.008548372943871894100, 0.008843099835763678848, 0.009137826727655463596, 0.009432553619547248344 ),
 .UNSPECIFIED. ) ;
#1218 = DIRECTION ( 'NONE',  ( 1.000000000000000000, 0.000000000000000000, 0.000000000000000000 ) ) ;
#1219 = CARTESIAN_POINT ( 'NONE',  ( -6.877134118866000456, -50.00000000000000000, 5.285102517561346858 ) ) ;
#1220 = DIRECTION ( 'NONE',  ( -1.000000000000000000, 0.000000000000000000, 0.000000000000000000 ) ) ;
#1221 = DIRECTION ( 'NONE',  ( 0.000000000000000000, 0.000000000000000000, 1.000000000000000000 ) ) ;
#1222 = CARTESIAN_POINT ( 'NONE',  ( 4.962858103399386600, -73.37410943649805972, 0.6966535907275263062 ) ) ;
#1223 = CARTESIAN_POINT ( 'NONE',  ( 0.000000000000000000, -72.50000000000001421, -2.500000000000000444 ) ) ;
#1224 = CARTESIAN_POINT ( 'NONE',  ( -11.03470001049179494, -52.79999999999999716, 2.958453039083849045 ) ) ;
#1225 = CARTESIAN_POINT ( 'NONE',  ( 7.005833569765714586, -50.00000000000000000, 9.116201041261451365 ) ) ;
#1226 = CARTESIAN_POINT ( 'NONE',  ( -11.03475136337292639, -50.94770623811574239, -1.034751363372938160 ) ) ;
#1227 = CARTESIAN_POINT ( 'NONE',  ( 11.39999999999999680, -52.79999999999999716, -1.639999999999997460 ) ) ;
#1228 = ORIENTED_EDGE ( 'NONE', *, *, #1967, .F. ) ;
#1229 = CARTESIAN_POINT ( 'NONE',  ( 7.513445500750180805, -50.00000000000000000, 4.333070140107198043 ) ) ;
#1230 = EDGE_CURVE ( 'NONE', #2520, #2101, #1217, .T. ) ;
#1231 = CARTESIAN_POINT ( 'NONE',  ( 4.481108542057384625, -6.016226048536217341, -2.241414944841849888 ) ) ;
#1232 = CYLINDRICAL_SURFACE ( 'NONE', #794, 2.500000000000000444 ) ;
#1233 = CARTESIAN_POINT ( 'NONE',  ( -11.39999999999999680, -47.20000000000001705, -1.639999999999997460 ) ) ;
#1234 = CARTESIAN_POINT ( 'NONE',  ( -11.40000000000000036, -49.88862030549578463, -1.400000000000000355 ) ) ;
#1235 = ORIENTED_EDGE ( 'NONE', *, *, #2947, .F. ) ;
#1236 = SHAPE_REPRESENTATION ( 'connecting link', ( #1692 ), #2651 ) ;
#1237 = CARTESIAN_POINT ( 'NONE',  ( 9.920087608940491464, -51.40000000000001279, 0.07988930269788889482 ) ) ;
#1238 = CARTESIAN_POINT ( 'NONE',  ( 9.116201041288118034, -52.79999999999999716, 7.005833569791843907 ) ) ;
#1239 = CARTESIAN_POINT ( 'NONE',  ( 5.742338339643763945, -50.00000000000000000, 9.960716663318306630 ) ) ;
#1240 = DIRECTION ( 'NONE',  ( 0.000000000000000000, 0.000000000000000000, 1.000000000000000000 ) ) ;
#1241 = CARTESIAN_POINT ( 'NONE',  ( -8.599999999999996092, -52.79999999999999716, -1.639999999999997460 ) ) ;
#1242 = ORIENTED_EDGE ( 'NONE', *, *, #558, .F. ) ;
#1243 = CARTESIAN_POINT ( 'NONE',  ( -6.877134118866001344, -47.20000000000001705, 5.285102517561345969 ) ) ;
#1244 = PRODUCT_CONTEXT ( 'NONE', #3220, 'mechanical' ) ;
#1245 = CARTESIAN_POINT ( 'NONE',  ( -3.117018002318639347, -64.86457393883293321, 3.922457828541068281 ) ) ;
#1246 = AXIS2_PLACEMENT_3D ( 'NONE', #3052, #43, #1749 ) ;
#1247 = CARTESIAN_POINT ( 'NONE',  ( 4.716912583111714241, -66.29091800361955222, 1.666493794562607711 ) ) ;
#1248 = VECTOR ( 'NONE', #2015, 1000.000000000000000 ) ;
#1249 = CARTESIAN_POINT ( 'NONE',  ( 0.000000000000000000, -80.00000000000000000, 0.000000000000000000 ) ) ;
#1250 = CARTESIAN_POINT ( 'NONE',  ( -0.3000000000000161982, -118.9999999999982379, -0.7416198487096117287 ) ) ;
#1251 = FACE_OUTER_BOUND ( 'NONE', #520, .T. ) ;
#1252 = VECTOR ( 'NONE', #1034, 1000.000000000000000 ) ;
#1253 = CARTESIAN_POINT ( 'NONE',  ( 11.39999532361432522, -52.79999999999999716, 0.1755699507458462760 ) ) ;
#1254 = CARTESIAN_POINT ( 'NONE',  ( 11.37702123033542279, -50.00000000000000000, 0.7471912688806704450 ) ) ;
#1255 =( LENGTH_UNIT ( ) NAMED_UNIT ( * ) SI_UNIT ( .MILLI., .METRE. ) );
#1256 = CARTESIAN_POINT ( 'NONE',  ( -8.582665138674013150, -50.00000000000000000, 0.5636706063486749407 ) ) ;
#1257 = ORIENTED_EDGE ( 'NONE', *, *, #2988, .T. ) ;
#1258 = CARTESIAN_POINT ( 'NONE',  ( 4.997074555615626856, -51.49033316323540532, -0.1965204501117691904 ) ) ;
#1259 = CARTESIAN_POINT ( 'NONE',  ( 3.320170879781855433, -6.729821324027721374, 3.751849819826997834 ) ) ;
#1260 = VECTOR ( 'NONE', #1699, 1000.000000000000000 ) ;
#1261 = CARTESIAN_POINT ( 'NONE',  ( -4.871060595381011993, -50.99085979125018753, 1.130390421582378124 ) ) ;
#1262 = UNCERTAINTY_MEASURE_WITH_UNIT (LENGTH_MEASURE( 1.000000000000000082E-05 ), #132, 'distance_accuracy_value', 'NONE');
#1263 = CARTESIAN_POINT ( 'NONE',  ( -9.999999999999998224, -48.60000000000000142, 1.734719587726169024E-19 ) ) ;
#1264 = FACE_OUTER_BOUND ( 'NONE', #3204, .T. ) ;
#1265 = CIRCLE ( 'NONE', #263, 1.499999999999999778 ) ;
#1266 = CARTESIAN_POINT ( 'NONE',  ( 0.000000000000000000, 0.000000000000000000, 0.000000000000000000 ) ) ;
#1267 = CARTESIAN_POINT ( 'NONE',  ( 0.000000000000000000, 0.000000000000000000, 18.00000000000000355 ) ) ;
#1268 = CARTESIAN_POINT ( 'NONE',  ( 8.489369361306732031, -50.00000000000000000, 1.403517616196621409 ) ) ;
#1269 = ORIENTED_EDGE ( 'NONE', *, *, #2510, .T. ) ;
#1270 =( NAMED_UNIT ( * ) PLANE_ANGLE_UNIT ( ) SI_UNIT ( $, .RADIAN. ) );
#1271 = CARTESIAN_POINT ( 'NONE',  ( 1.181079518071022826E-19, -64.00000000000000000, 4.999999999999999112 ) ) ;
#1272 = EDGE_CURVE ( 'NONE', #2870, #3130, #3268, .T. ) ;
#1273 = DIRECTION ( 'NONE',  ( 0.000000000000000000, 0.000000000000000000, 1.000000000000000000 ) ) ;
#1274 = DIRECTION ( 'NONE',  ( 0.000000000000000000, 1.000000000000000000, 0.000000000000000000 ) ) ;
#1275 = ORIENTED_EDGE ( 'NONE', *, *, #2410, .T. ) ;
#1276 = DIRECTION ( 'NONE',  ( -0.000000000000000000, 1.000000000000000000, -0.000000000000000000 ) ) ;
#1277 = ITEM_DEFINED_TRANSFORMATION ( 'NONE', 'NONE', #1117,  #1692 ) ;
#1278 = CARTESIAN_POINT ( 'NONE',  ( -3.791988745706118102, -65.34238691411069055, 3.273615902745505846 ) ) ;
#1279 = CARTESIAN_POINT ( 'NONE',  ( -4.916101592540525367, -51.19835914624871975, -0.9229043554563169938 ) ) ;
#1280 = FACE_OUTER_BOUND ( 'NONE', #3189, .T. ) ;
#1281 = DIRECTION ( 'NONE',  ( -0.000000000000000000, -1.000000000000000000, -0.000000000000000000 ) ) ;
#1282 = CARTESIAN_POINT ( 'NONE',  ( 8.502540660504635639, -50.22987518539597573, 1.385387373903631314 ) ) ;
#1283 = CARTESIAN_POINT ( 'NONE',  ( 8.582665138674004268, -50.00000000000000000, 0.5636706063485154017 ) ) ;
#1284 = ORIENTED_EDGE ( 'NONE', *, *, #156, .F. ) ;
#1285 = EDGE_CURVE ( 'NONE', #1384, #1132, #1725, .T. ) ;
#1286 = PRESENTATION_STYLE_ASSIGNMENT (( #551 ) ) ;
#1287 = CARTESIAN_POINT ( 'NONE',  ( 8.572527594031472993E-15, -70.00000000000000000, 0.000000000000000000 ) ) ;
#1288 = CARTESIAN_POINT ( 'NONE',  ( -3.321910197521175778, -6.728960966335735705, 3.750313380908745664 ) ) ;
#1289 = EDGE_CURVE ( 'NONE', #1132, #721, #1291, .T. ) ;
#1290 = VERTEX_POINT ( 'NONE', #1611 ) ;
#1291 = LINE ( 'NONE', #2306, #775 ) ;
#1292 = CARTESIAN_POINT ( 'NONE',  ( 7.513445500750181694, -47.20000000000001705, 4.333070140107198043 ) ) ;
#1293 = EDGE_LOOP ( 'NONE', ( #1388, #2887, #514, #3110, #2636, #1559 ) ) ;
#1294 = ADVANCED_FACE ( 'NONE', ( #2627 ), #2915, .F. ) ;
#1295 = CARTESIAN_POINT ( 'NONE',  ( -3.359134405502826048, -74.97878567386173643, 3.716361166143389294 ) ) ;
#1296 = FACE_OUTER_BOUND ( 'NONE', #1082, .T. ) ;
#1297 = PRODUCT_DEFINITION ( 'UNKNOWN', '', #1325, #1531 ) ;
#1298 = CARTESIAN_POINT ( 'NONE',  ( -3.854351720261343002E-15, -119.2999999999982776, -0.7850000000000663114 ) ) ;
#1299 = AXIS2_PLACEMENT_3D ( 'NONE', #2521, #1276, #2585 ) ;
#1300 = FACE_OUTER_BOUND ( 'NONE', #1135, .T. ) ;
#1301 = CARTESIAN_POINT ( 'NONE',  ( -8.582665138674013150, -50.00000000000000000, 0.5636706063486749407 ) ) ;
#1302 = ORIENTED_EDGE ( 'NONE', *, *, #966, .F. ) ;
#1303 = CLOSED_SHELL ( 'NONE', ( #407, #2732, #1733, #1166, #1023, #1880, #2511, #56, #2264, #253, #835, #1397, #1438, #659, #1294, #2491 ) ) ;
#1304 = SURFACE_SIDE_STYLE ('',( #2038 ) ) ;
#1305 = PRESENTATION_STYLE_ASSIGNMENT (( #3112 ) ) ;
#1306 = AXIS2_PLACEMENT_3D ( 'NONE', #1060, #2108, #3115 ) ;
#1307 = CARTESIAN_POINT ( 'NONE',  ( -8.530791689320901483, -50.00000000000000000, 1.124695299888049504 ) ) ;
#1308 = LINE ( 'NONE', #299, #2827 ) ;
#1309 = ORIENTED_EDGE ( 'NONE', *, *, #156, .T. ) ;
#1310 = CARTESIAN_POINT ( 'NONE',  ( 4.996981400519024952, -51.49002086460089345, 0.1986267936440539450 ) ) ;
#1311 = CONTEXT_DEPENDENT_SHAPE_REPRESENTATION ( #2040, #2398 ) ;
#1312 = EDGE_CURVE ( 'NONE', #1786, #2825, #3263, .T. ) ;
#1313 = CARTESIAN_POINT ( 'NONE',  ( -11.40000778997679198, -47.20000000000001705, -0.2924664341913127408 ) ) ;
#1314 = CARTESIAN_POINT ( 'NONE',  ( -4.927416625552392127, -73.42405444405065396, 0.8653657731671230424 ) ) ;
#1315 = DIRECTION ( 'NONE',  ( -0.000000000000000000, -0.000000000000000000, 1.000000000000000000 ) ) ;
#1316 = ORIENTED_EDGE ( 'NONE', *, *, #2514, .T. ) ;
#1317 = DIRECTION ( 'NONE',  ( -1.000000000000000000, 0.000000000000000000, 0.000000000000000000 ) ) ;
#1318 = CARTESIAN_POINT ( 'NONE',  ( -8.572276570256935457, -52.79999999999999716, 0.7042094815226510596 ) ) ;
#1319 = VECTOR ( 'NONE', #2742, 1000.000000000000000 ) ;
#1320 = VERTEX_POINT ( 'NONE', #1394 ) ;
#1321 = CARTESIAN_POINT ( 'NONE',  ( 2.300000000000000266, -67.40000000000000568, -1.734723475976807094E-15 ) ) ;
#1322 = AXIS2_PLACEMENT_3D ( 'NONE', #708, #781, #2215 ) ;
#1323 = CARTESIAN_POINT ( 'NONE',  ( 8.489369361306732031, -50.00000000000000000, 1.403517616196621409 ) ) ;
#1324 = CARTESIAN_POINT ( 'NONE',  ( 5.285102517541700351, -50.00000000000000000, 6.877134118846478295 ) ) ;
#1325 = PRODUCT_DEFINITION_FORMATION_WITH_SPECIFIED_SOURCE ( 'ANY', '', #862, .NOT_KNOWN. ) ;
#1326 = ORIENTED_EDGE ( 'NONE', *, *, #2132, .T. ) ;
#1327 = CARTESIAN_POINT ( 'NONE',  ( 4.945771905224659371, -51.30991108704697012, -0.7565992915569080823 ) ) ;
#1328 = CARTESIAN_POINT ( 'NONE',  ( -9.959683570761574956, -47.20000000000001705, 5.743837162464267898 ) ) ;
#1329 = ORIENTED_EDGE ( 'NONE', *, *, #1029, .T. ) ;
#1330 = EDGE_CURVE ( 'NONE', #2538, #2574, #353, .T. ) ;
#1331 = DIRECTION ( 'NONE',  ( -0.000000000000000000, -0.000000000000000000, 1.000000000000000000 ) ) ;
#1332 = CARTESIAN_POINT ( 'NONE',  ( -8.324422814933019055, -50.00000000000000000, 2.231815450536601464 ) ) ;
#1333 = VERTEX_POINT ( 'NONE', #1890 ) ;
#1334 = CARTESIAN_POINT ( 'NONE',  ( 6.123233995736765296E-16, -80.00000000000000000, -4.999999999999999112 ) ) ;
#1335 = CARTESIAN_POINT ( 'NONE',  ( -8.599996472200352571, -50.00000000000000000, 0.1525981975067654262 ) ) ;
#1336 = ORIENTED_EDGE ( 'NONE', *, *, #2260, .T. ) ;
#1337 = CYLINDRICAL_SURFACE ( 'NONE', #3067, 2.499999999999999556 ) ;
#1338 = CARTESIAN_POINT ( 'NONE',  ( 4.999850703040199740, 5.590303478919644853, 0.1739517833579089512 ) ) ;
#1339 = CARTESIAN_POINT ( 'NONE',  ( 1.181079518071022826E-19, -64.00000000000000000, 4.999999999999999112 ) ) ;
#1340 = CARTESIAN_POINT ( 'NONE',  ( 8.452889752740453844, -50.00000000000000000, 1.586704117746243314 ) ) ;
#1341 = ORIENTED_EDGE ( 'NONE', *, *, #1643, .T. ) ;
#1342 = CARTESIAN_POINT ( 'NONE',  ( -3.772047191027663615, 6.487346954507292374, -3.297239103104800506 ) ) ;
#1343 = CARTESIAN_POINT ( 'NONE',  ( 8.599999999999996092, -47.20000000000001705, -1.093333333333372126 ) ) ;
#1344 = B_SPLINE_CURVE_WITH_KNOTS ( 'NONE', 3,
 ( #2501, #2022, #3034, #2759 ),
 .UNSPECIFIED., .F., .F.,
 ( 4, 4 ),
 ( 0.005006932180914174663, 0.009012567534305281416 ),
 .UNSPECIFIED. ) ;
#1345 = APPLICATION_CONTEXT ( 'automotive_design' ) ;
#1346 = ORIENTED_EDGE ( 'NONE', *, *, #473, .T. ) ;
#1347 = CARTESIAN_POINT ( 'NONE',  ( 4.999999999999999112, -66.68337520964459486, 0.000000000000000000 ) ) ;
#1348 = CARTESIAN_POINT ( 'NONE',  ( -4.331939449206426929, -50.00000000000000000, 7.514224851276241957 ) ) ;
#1349 = VERTEX_POINT ( 'NONE', #3168 ) ;
#1350 =( NAMED_UNIT ( * ) PLANE_ANGLE_UNIT ( ) SI_UNIT ( $, .RADIAN. ) );
#1351 = DIRECTION ( 'NONE',  ( 0.000000000000000000, 0.000000000000000000, 1.000000000000000000 ) ) ;
#1352 = CARTESIAN_POINT ( 'NONE',  ( 9.920079092145082100, -48.60000000000001563, 0.07989781697635986446 ) ) ;
#1353 = ORIENTED_EDGE ( 'NONE', *, *, #1965, .T. ) ;
#1354 = COLOUR_RGB ( '',0.8941176470588234615, 0.8941176470588234615, 0.8941176470588234615 ) ;
#1355 = FACE_OUTER_BOUND ( 'NONE', #183, .T. ) ;
#1356 = CARTESIAN_POINT ( 'NONE',  ( 0.000000000000000000, 0.000000000000000000, 0.000000000000000000 ) ) ;
#1357 = CARTESIAN_POINT ( 'NONE',  ( 3.077296587540346184, 6.845542784947758364, -3.953776968828220717 ) ) ;
#1358 = CARTESIAN_POINT ( 'NONE',  ( -4.962858103399387488, -66.62589056350195449, 0.6966535907275258621 ) ) ;
#1359 = CARTESIAN_POINT ( 'NONE',  ( -4.990888858476322021, -5.598354044414833197, 0.3458703032855571791 ) ) ;
#1360 = ORIENTED_EDGE ( 'NONE', *, *, #1175, .F. ) ;
#1361 = CARTESIAN_POINT ( 'NONE',  ( 1.836970198721029688E-16, -125.0000000000000000, -1.499999999999999778 ) ) ;
#1362 = CARTESIAN_POINT ( 'NONE',  ( -11.39999532361432522, -52.79999999999999716, 0.1755699507458657049 ) ) ;
#1363 = ORIENTED_EDGE ( 'NONE', *, *, #528, .F. ) ;
#1364 =( BOUNDED_CURVE ( )  B_SPLINE_CURVE ( 3, ( #2220, #1187, #2959, #2483 ),
 .UNSPECIFIED., .F., .T. ) 
 B_SPLINE_CURVE_WITH_KNOTS ( ( 4, 4 ),
 ( 3.141592653589791340, 4.712388980384689674 ),
 .UNSPECIFIED. ) 
 CURVE ( )  GEOMETRIC_REPRESENTATION_ITEM ( )  RATIONAL_B_SPLINE_CURVE ( ( 1.000000000000000000, 0.8047378541243646044, 0.8047378541243646044, 1.000000000000000000 ) ) 
 REPRESENTATION_ITEM ( '' )  );
#1365 = CARTESIAN_POINT ( 'NONE',  ( -4.999999999999999112, -73.31662479035540514, 0.000000000000000000 ) ) ;
#1366 = CARTESIAN_POINT ( 'NONE',  ( 2.250215587473118450, -50.00000000000000000, 8.376503107919017310 ) ) ;
#1367 = ORIENTED_EDGE ( 'NONE', *, *, #697, .T. ) ;
#1368 = DIRECTION ( 'NONE',  ( 0.000000000000000000, 0.000000000000000000, 1.000000000000000000 ) ) ;
#1369 = PLANE ( 'NONE',  #2105 ) ;
#1370 = CARTESIAN_POINT ( 'NONE',  ( 8.599999999999996092, -50.00000000000000000, -1.093333333333372126 ) ) ;
#1371 = EDGE_LOOP ( 'NONE', ( #885, #2968, #1275, #1228, #2310, #139 ) ) ;
#1372 = CIRCLE ( 'NONE', #2168, 4.999999999999999112 ) ;
#1373 = ADVANCED_FACE ( 'NONE', ( #2093 ), #85, .F. ) ;
#1374 = DIRECTION ( 'NONE',  ( -1.000000000000000000, 0.000000000000000000, 0.000000000000000000 ) ) ;
#1375 = AXIS2_PLACEMENT_3D ( 'NONE', #2936, #2973, #934 ) ;
#1376 = CARTESIAN_POINT ( 'NONE',  ( 0.000000000000000000, 7.500000000000000000, 4.999999999999999112 ) ) ;
#1377 = CARTESIAN_POINT ( 'NONE',  ( -2.982843918280285944, -47.20000000000001705, 11.10373667793902541 ) ) ;
#1378 = B_SPLINE_CURVE_WITH_KNOTS ( 'NONE', 3,
 ( #99, #1106, #366, #1126 ),
 .UNSPECIFIED., .F., .F.,
 ( 4, 4 ),
 ( 0.005008082645073257469, 0.009013720360685723715 ),
 .UNSPECIFIED. ) ;
#1379 =( GEOMETRIC_REPRESENTATION_CONTEXT ( 3 ) GLOBAL_UNCERTAINTY_ASSIGNED_CONTEXT ( ( #1501 ) ) GLOBAL_UNIT_ASSIGNED_CONTEXT ( ( #2622, #2894, #880 ) ) REPRESENTATION_CONTEXT ( 'NONE', 'WORKASPACE' ) );
#1380 = CARTESIAN_POINT ( 'NONE',  ( -0.3368283383274193743, 7.494339828221662003, -4.991522157455978714 ) ) ;
#1381 = CARTESIAN_POINT ( 'NONE',  ( -11.30825875095987421, -52.79999999999999716, 1.490875164968288757 ) ) ;
#1382 = VERTEX_POINT ( 'NONE', #1657 ) ;
#1383 = CARTESIAN_POINT ( 'NONE',  ( 0.000000000000000000, 80.00000000000000000, 0.000000000000000000 ) ) ;
#1384 = VERTEX_POINT ( 'NONE', #2130 ) ;
#1385 = CARTESIAN_POINT ( 'NONE',  ( 2.499999999999999556, 0.000000000000000000, 18.00000000000000355 ) ) ;
#1386 = CARTESIAN_POINT ( 'NONE',  ( 4.999999999999999112, -80.00000000000000000, 0.000000000000000000 ) ) ;
#1387 = CARTESIAN_POINT ( 'NONE',  ( 0.3332490247102218861, -67.51676079561944732, -4.991558521926720005 ) ) ;
#1388 = ORIENTED_EDGE ( 'NONE', *, *, #507, .F. ) ;
#1389 = CARTESIAN_POINT ( 'NONE',  ( 2.500000000000004441, -70.00000000000000000, 0.000000000000000000 ) ) ;
#1390 =( NAMED_UNIT ( * ) SI_UNIT ( $, .STERADIAN. ) SOLID_ANGLE_UNIT ( ) );
#1391 = EDGE_CURVE ( 'NONE', #74, #277, #3137, .T. ) ;
#1392 = CARTESIAN_POINT ( 'NONE',  ( -11.39999999999999680, -50.00000000000000000, -0.5466666666666361030 ) ) ;
#1393 = CARTESIAN_POINT ( 'NONE',  ( -11.39999999999999680, -50.00000000000000000, -1.013333333333681141 ) ) ;
#1394 = CARTESIAN_POINT ( 'NONE',  ( -5.000000000000000000, 24.40983005625052726, 18.00000000000000355 ) ) ;
#1395 = CARTESIAN_POINT ( 'NONE',  ( -11.03470001049179494, -52.79999999999999716, 2.958453039083849045 ) ) ;
#1396 = EDGE_CURVE ( 'NONE', #84, #1895, #1536, .T. ) ;
#1397 = ADVANCED_FACE ( 'NONE', ( #911 ), #2180, .F. ) ;
#1398 = EDGE_LOOP ( 'NONE', ( #3116, #1814, #1901, #2273, #168, #1666 ) ) ;
#1399 = DIRECTION ( 'NONE',  ( 0.000000000000000000, 0.000000000000000000, 1.000000000000000000 ) ) ;
#1400 = ORIENTED_EDGE ( 'NONE', *, *, #1118, .F. ) ;
#1401 = ADVANCED_BREP_SHAPE_REPRESENTATION ( '', ( #1612, #1692 ), #1379 ) ;
#1402 = CARTESIAN_POINT ( 'NONE',  ( 0.000000000000000000, 0.000000000000000000, -10.00000000000000000 ) ) ;
#1403 = CARTESIAN_POINT ( 'NONE',  ( -0.3000000000000161982, -114.9999999999982236, 0.9539392014169767453 ) ) ;
#1404 = ORIENTED_EDGE ( 'NONE', *, *, #1442, .T. ) ;
#1405 = CARTESIAN_POINT ( 'NONE',  ( -1.464466094067257806, -72.50000000000001421, 2.499999999999999556 ) ) ;
#1406 = SURFACE_SIDE_STYLE ('',( #1886 ) ) ;
#1407 = CARTESIAN_POINT ( 'NONE',  ( -11.36325033731739076, -47.20000000000001705, 0.9334869871344717573 ) ) ;
#1408 = CARTESIAN_POINT ( 'NONE',  ( -7.005833569765055557, -50.00000000000000000, 9.116201041262108618 ) ) ;
#1409 = COLOUR_RGB ( '',0.8941176470588234615, 0.8941176470588234615, 0.8941176470588234615 ) ;
#1410 = CARTESIAN_POINT ( 'NONE',  ( -0.3000000000000161982, -118.9999999999982379, -2.300000000000000266 ) ) ;
#1411 = MECHANICAL_DESIGN_GEOMETRIC_PRESENTATION_REPRESENTATION (  '', ( #982 ), #1197 ) ;
#1412 = CARTESIAN_POINT ( 'NONE',  ( 11.03470001049119453, -50.00000000000000000, 2.958453039085983338 ) ) ;
#1413 = ORIENTED_EDGE ( 'NONE', *, *, #303, .T. ) ;
#1414 = EDGE_CURVE ( 'NONE', #1621, #229, #2012, .T. ) ;
#1415 = CARTESIAN_POINT ( 'NONE',  ( 0.000000000000000000, 0.000000000000000000, 18.00000000000000355 ) ) ;
#1416 = CIRCLE ( 'NONE', #521, 1.499999999999999778 ) ;
#1417 = PLANE ( 'NONE',  #2961 ) ;
#1418 = ORIENTED_EDGE ( 'NONE', *, *, #2173, .F. ) ;
#1419 = CARTESIAN_POINT ( 'NONE',  ( 8.599999999999996092, -50.00000000000000000, -1.093333333333372126 ) ) ;
#1420 = CARTESIAN_POINT ( 'NONE',  ( 6.122861072698252249E-16, -67.50000000000000000, -4.999999999999999112 ) ) ;
#1421 = ORIENTED_EDGE ( 'NONE', *, *, #1153, .T. ) ;
#1422 = DIRECTION ( 'NONE',  ( 0.000000000000000000, 0.000000000000000000, 1.000000000000000000 ) ) ;
#1423 = CARTESIAN_POINT ( 'NONE',  ( 7.005833569766282132, -47.20000000000001705, 9.116201041261453142 ) ) ;
#1424 = AXIS2_PLACEMENT_3D ( 'NONE', #3226, #237, #207 ) ;
#1425 = CARTESIAN_POINT ( 'NONE',  ( -0.8424979979451828749, -7.454395415945072045, -4.931395878866434046 ) ) ;
#1426 = CARTESIAN_POINT ( 'NONE',  ( -9.920087608911693167, -51.39999999999999858, 0.07988930266963500948 ) ) ;
#1427 = CIRCLE ( 'NONE', #2849, 2.300000000000000266 ) ;
#1428 = CARTESIAN_POINT ( 'NONE',  ( 11.39999999999999680, -50.00000000000000000, -1.366666666666861873 ) ) ;
#1429 = ORIENTED_EDGE ( 'NONE', *, *, #1474, .F. ) ;
#1430 = CARTESIAN_POINT ( 'NONE',  ( -8.324422814933019055, -47.20000000000001705, 2.231815450536601020 ) ) ;
#1431 = CARTESIAN_POINT ( 'NONE',  ( 2.300000000000000266, -72.60000000000000853, 0.000000000000000000 ) ) ;
#1432 = CARTESIAN_POINT ( 'NONE',  ( 8.572527594031472993E-15, -70.00000000000000000, 10.00000000000000000 ) ) ;
#1433 = EDGE_LOOP ( 'NONE', ( #2607, #308 ) ) ;
#1434 = CARTESIAN_POINT ( 'NONE',  ( 4.954123618475600566, -66.61507573143732941, 0.6974948150963297122 ) ) ;
#1435 = CARTESIAN_POINT ( 'NONE',  ( 1.125736483476999839, -50.00000000000000000, 8.599999999999996092 ) ) ;
#1436 = CARTESIAN_POINT ( 'NONE',  ( -11.33515354614430670, -49.56496474501410887, -1.335153546144310699 ) ) ;
#1437 = CARTESIAN_POINT ( 'NONE',  ( 10.31604092329498989, -51.37342103705936580, -0.3160374682705313631 ) ) ;
#1438 = ADVANCED_FACE ( 'NONE', ( #2471 ), #719, .F. ) ;
#1439 = CARTESIAN_POINT ( 'NONE',  ( -4.815309899926791815, -49.33271645601669775, -1.346969744587360074 ) ) ;
#1440 = CARTESIAN_POINT ( 'NONE',  ( 2.982843918280841500, -47.20000000000001705, 11.10373667793903074 ) ) ;
#1441 = CARTESIAN_POINT ( 'NONE',  ( -0.3000000000000161982, -114.9999999999982236, 0.9539392014169767453 ) ) ;
#1442 = EDGE_CURVE ( 'NONE', #2378, #890, #2873, .T. ) ;
#1443 = CARTESIAN_POINT ( 'NONE',  ( -10.62090117298859759, -51.26516722440712925, -0.6209000891238662945 ) ) ;
#1444 = CARTESIAN_POINT ( 'NONE',  ( 11.39999999999999680, -52.79999999999999716, -1.093333333333372126 ) ) ;
#1445 = ORIENTED_EDGE ( 'NONE', *, *, #1312, .F. ) ;
#1446 = CARTESIAN_POINT ( 'NONE',  ( -8.489369361306263073, -50.00000000000000000, 1.403517616197273554 ) ) ;
#1447 = CARTESIAN_POINT ( 'NONE',  ( 0.000000000000000000, 0.000000000000000000, -10.00000000000000000 ) ) ;
#1448 = ORIENTED_EDGE ( 'NONE', *, *, #983, .T. ) ;
#1449 = LINE ( 'NONE', #951, #2117 ) ;
#1450 = CARTESIAN_POINT ( 'NONE',  ( 6.877134118866902845, -50.00000000000000000, 5.285102517562147995 ) ) ;
#1451 = DIRECTION ( 'NONE',  ( -0.000000000000000000, -0.000000000000000000, -1.000000000000000000 ) ) ;
#1452 = CARTESIAN_POINT ( 'NONE',  ( -0.3000000000000161982, -118.9999999999982379, -0.7416198487096117287 ) ) ;
#1453 = LINE ( 'NONE', #2174, #1105 ) ;
#1454 = CARTESIAN_POINT ( 'NONE',  ( 2.982843918280273510, -50.00000000000000000, 11.10373667793903252 ) ) ;
#1455 = CARTESIAN_POINT ( 'NONE',  ( 11.39999999999999680, -50.00000000000000000, -1.206666666669127919 ) ) ;
#1456 = FACE_BOUND ( 'NONE', #2903, .T. ) ;
#1457 = EDGE_CURVE ( 'NONE', #439, #1320, #243, .T. ) ;
#1458 = CARTESIAN_POINT ( 'NONE',  ( 8.582665138674004268, -52.79999999999999716, 0.5636706063485154017 ) ) ;
#1459 = ORIENTED_EDGE ( 'NONE', *, *, #2588, .T. ) ;
#1460 = CARTESIAN_POINT ( 'NONE',  ( -8.599996472200352571, -47.20000000000001705, 0.1525981975067654817 ) ) ;
#1461 = CIRCLE ( 'NONE', #2207, 2.500000000000000000 ) ;
#1462 = CARTESIAN_POINT ( 'NONE',  ( 0.6557238592495003848, -72.41814643914202065, -4.959498321622188399 ) ) ;
#1463 = CARTESIAN_POINT ( 'NONE',  ( 0.1683266833682984520, -7.500000000000003553, -5.000000000000000000 ) ) ;
#1464 = ORIENTED_EDGE ( 'NONE', *, *, #528, .T. ) ;
#1465 = APPLICATION_CONTEXT ( 'automotive_design' ) ;
#1466 = CARTESIAN_POINT ( 'NONE',  ( 4.999999999999999112, -66.68337520964459486, 0.000000000000000000 ) ) ;
#1467 = CIRCLE ( 'NONE', #3267, 6.000000000000001776 ) ;
#1468 = CARTESIAN_POINT ( 'NONE',  ( -4.331939449206426929, -50.00000000000000000, 7.514224851276241957 ) ) ;
#1469 = CARTESIAN_POINT ( 'NONE',  ( -2.500000000000000000, 3.061616997868383141E-16, 18.00000000000000355 ) ) ;
#1470 = FACE_OUTER_BOUND ( 'NONE', #3250, .T. ) ;
#1471 = DIRECTION ( 'NONE',  ( 0.000000000000000000, 1.000000000000000000, 0.000000000000000000 ) ) ;
#1472 = CARTESIAN_POINT ( 'NONE',  ( -11.39999999999999680, -52.79999999999999716, -1.093333333333363022 ) ) ;
#1473 = CARTESIAN_POINT ( 'NONE',  ( 4.856148773929144902, -49.08427523399102910, 1.192039989181127080 ) ) ;
#1474 = EDGE_CURVE ( 'NONE', #2378, #661, #2444, .T. ) ;
#1475 = CARTESIAN_POINT ( 'NONE',  ( 0.000000000000000000, -114.9999999999982236, -2.300000000000000266 ) ) ;
#1476 = CARTESIAN_POINT ( 'NONE',  ( 11.37702123033549384, -52.79999999999999716, 0.7471912688806703340 ) ) ;
#1477 = EDGE_CURVE ( 'NONE', #1754, #2538, #2569, .T. ) ;
#1478 = ORIENTED_EDGE ( 'NONE', *, *, #1147, .F. ) ;
#1479 = VECTOR ( 'NONE', #1451, 1000.000000000000000 ) ;
#1480 = CARTESIAN_POINT ( 'NONE',  ( -4.331939449206426929, -50.00000000000000000, 7.514224851276241957 ) ) ;
#1481 = AXIS2_PLACEMENT_3D ( 'NONE', #1679, #2953, #693 ) ;
#1482 = CARTESIAN_POINT ( 'NONE',  ( 11.29810924534245231, -49.46572717680115261, -1.298109245342459639 ) ) ;
#1483 = EDGE_CURVE ( 'NONE', #14, #1349, #2721, .T. ) ;
#1484 = CIRCLE ( 'NONE', #745, 2.300000000000000266 ) ;
#1485 = DIRECTION ( 'NONE',  ( 0.000000000000000000, 1.000000000000000000, 0.000000000000000000 ) ) ;
#1486 = CARTESIAN_POINT ( 'NONE',  ( 8.582665138674004268, -47.20000000000001705, 0.5636706063485154017 ) ) ;
#1487 = B_SPLINE_CURVE_WITH_KNOTS ( 'NONE', 3,
 ( #188, #173, #1932, #3205, #1697, #2218, #1681, #2461, #1185, #1201, #1500, #1711, #428, #3221, #1728, #2509, #1247, #679, #2696, #2714, #1434, #2200, #1950, #1466 ),
 .UNSPECIFIED., .F., .F.,
 ( 4, 2, 2, 2, 2, 2, 2, 2, 2, 2, 2, 4 ),
 ( 0.008369288751650572414, 0.008891570837864926427, 0.009413852924079280440, 0.01045841709650799541, 0.01150298126893671211, 0.01254754544136542707, 0.01359210961379414551, 0.01463667378622286047, 0.01515895587243720928, 0.01568123795865155809, 0.01620352004486590863, 0.01672580213108025918 ),
 .UNSPECIFIED. ) ;
#1488 = CARTESIAN_POINT ( 'NONE',  ( 0.000000000000000000, 0.000000000000000000, 10.00000000000000000 ) ) ;
#1489 = AXIS2_PLACEMENT_3D ( 'NONE', #1266, #3033, #3086 ) ;
#1490 = CARTESIAN_POINT ( 'NONE',  ( 10.76674801461901687, -51.18483196047734651, -0.7667480146190301937 ) ) ;
#1491 = CARTESIAN_POINT ( 'NONE',  ( 8.768448914935811800, -50.81504429929027822, 1.156277961913187990 ) ) ;
#1492 = CARTESIAN_POINT ( 'NONE',  ( 5.742338339643763945, -50.00000000000000000, 9.960716663318306630 ) ) ;
#1493 = CARTESIAN_POINT ( 'NONE',  ( 9.959683570760574867, -50.00000000000000000, 5.743837162466680191 ) ) ;
#1494 = FILL_AREA_STYLE_COLOUR ( '', #1354 ) ;
#1495 = ADVANCED_FACE ( 'NONE', ( #2706 ), #2687, .T. ) ;
#1496 = CARTESIAN_POINT ( 'NONE',  ( 7.005833569765147040, -52.79999999999999716, 9.116201041261453142 ) ) ;
#1497 = EDGE_LOOP ( 'NONE', ( #2982, #1646, #2810, #187, #3136, #645, #1781 ) ) ;
#1498 = CARTESIAN_POINT ( 'NONE',  ( 7.513445500750181694, -47.20000000000001705, 4.333070140107198043 ) ) ;
#1499 = CARTESIAN_POINT ( 'NONE',  ( 0.000000000000000000, -7.500000000000000000, 4.999999999999999112 ) ) ;
#1500 = CARTESIAN_POINT ( 'NONE',  ( 3.359134405502826048, -65.02121432613829199, 3.716361166143391959 ) ) ;
#1501 = UNCERTAINTY_MEASURE_WITH_UNIT (LENGTH_MEASURE( 1.000000000000000082E-05 ), #2622, 'distance_accuracy_value', 'NONE');
#1502 = DIRECTION ( 'NONE',  ( 1.000000000000000000, 0.000000000000000000, 0.000000000000000000 ) ) ;
#1503 = LINE ( 'NONE', #562, #988 ) ;
#1504 = DIRECTION ( 'NONE',  ( 0.000000000000000000, 0.000000000000000000, 1.000000000000000000 ) ) ;
#1505 = CARTESIAN_POINT ( 'NONE',  ( 11.39999999999999680, -50.00000000000000000, -1.366666666666861873 ) ) ;
#1506 = CARTESIAN_POINT ( 'NONE',  ( 4.977308113077120844, -48.57700265276938012, 0.4845947803478808380 ) ) ;
#1507 = CARTESIAN_POINT ( 'NONE',  ( -8.596526774713707297, -50.00000000000000000, 0.2821220414048196679 ) ) ;
#1508 = VERTEX_POINT ( 'NONE', #941 ) ;
#1509 = CARTESIAN_POINT ( 'NONE',  ( 4.985625624127048461, -51.45148266395612069, 0.3909128500499727821 ) ) ;
#1510 = CARTESIAN_POINT ( 'NONE',  ( 3.766216509439173965, -6.490735160851770047, 3.303865152441167297 ) ) ;
#1511 = VECTOR ( 'NONE', #2371, 1000.000000000000000 ) ;
#1512 = ADVANCED_FACE ( 'NONE', ( #1456, #197 ), #1209, .T. ) ;
#1513 = CARTESIAN_POINT ( 'NONE',  ( -4.772823807329270807, -50.19767535498903754, -1.490153625805560322 ) ) ;
#1514 = DIRECTION ( 'NONE',  ( -0.000000000000000000, -1.000000000000000000, 0.000000000000000000 ) ) ;
#1515 = FACE_BOUND ( 'NONE', #1065, .T. ) ;
#1516 = VECTOR ( 'NONE', #272, 1000.000000000000000 ) ;
#1517 = EDGE_CURVE ( 'NONE', #2753, #1195, #764, .T. ) ;
#1518 = B_SPLINE_CURVE_WITH_KNOTS ( 'NONE', 3,
 ( #2920, #2118, #1136, #3127, #598, #2416, #2677, #2871, #2648, #2167, #3176, #904, #648, #94, #2616, #861, #1915, #361 ),
 .UNSPECIFIED., .F., .F.,
 ( 4, 2, 2, 2, 2, 2, 2, 2, 4 ),
 ( 0.007951492273476376202, 0.008447850770476991039, 0.008944209267477605876, 0.009440567764478220714, 0.009936926261478833816, 0.01043328475847945039, 0.01092964325548006349, 0.01142600175248067833, 0.01192236024948129317 ),
 .UNSPECIFIED. ) ;
#1519 = DIRECTION ( 'NONE',  ( 0.000000000000000000, 0.000000000000000000, -1.000000000000000000 ) ) ;
#1520 = AXIS2_PLACEMENT_3D ( 'NONE', #3260, #2252, #512 ) ;
#1521 = CARTESIAN_POINT ( 'NONE',  ( -8.600005876649037262, -52.79999999999999716, -0.2541998246238979520 ) ) ;
#1522 = ORIENTED_EDGE ( 'NONE', *, *, #2781, .T. ) ;
#1523 = CARTESIAN_POINT ( 'NONE',  ( 2.368532205790481182, -70.81652027702884311, -4.403989053656482966 ) ) ;
#1524 = FACE_OUTER_BOUND ( 'NONE', #597, .T. ) ;
#1525 = CARTESIAN_POINT ( 'NONE',  ( 0.000000000000000000, -72.60000000000000853, 0.000000000000000000 ) ) ;
#1526 = ORIENTED_EDGE ( 'NONE', *, *, #3093, .F. ) ;
#1527 = CARTESIAN_POINT ( 'NONE',  ( 0.6733179620838674051, 7.471617105689219329, -4.957340513892267708 ) ) ;
#1528 = CARTESIAN_POINT ( 'NONE',  ( 4.324630367402185982, -6.131366064188266130, 2.529815037953009327 ) ) ;
#1529 = CIRCLE ( 'NONE', #2534, 2.300000000000000266 ) ;
#1530 = CARTESIAN_POINT ( 'NONE',  ( -1.181079518071022826E-19, -76.00000000000001421, 4.999999999999999112 ) ) ;
#1531 = PRODUCT_DEFINITION_CONTEXT ( 'detailed design', #279, 'design' ) ;
#1532 = AXIS2_PLACEMENT_3D ( 'NONE', #3270, #2029, #2372 ) ;
#1533 = EDGE_CURVE ( 'NONE', #14, #2794, #504, .T. ) ;
#1534 = LINE ( 'NONE', #3049, #476 ) ;
#1535 = CARTESIAN_POINT ( 'NONE',  ( 0.000000000000000000, -60.00000000000000000, -2.500000000000000444 ) ) ;
#1536 = B_SPLINE_CURVE_WITH_KNOTS ( 'NONE', 3,
 ( #1129, #1628, #1380, #2144, #2110, #1094, #625, #607, #2671, #1594, #2641, #1342, #2375, #103, #641, #3117, #1114, #871, #2897, #1837, #1872, #387, #133, #1143, #3151, #2609, #2845, #336, #2160, #370, #400, #2341, #591, #2395, #2357, #1642, #2656, #68, #1077, #3184 ),
 .UNSPECIFIED., .F., .F.,
 ( 4, 2, 2, 2, 2, 2, 2, 2, 2, 2, 2, 2, 2, 2, 2, 2, 2, 2, 2, 4 ),
 ( 0.01615986362459447684, 0.01666419217584455895, 0.01716852072709463758, 0.01817717782959479833, 0.01918583493209496255, 0.02019449203459512329, 0.02120314913709528404, 0.02221180623959544478, 0.02271613479084552342, 0.02322046334209560553, 0.02422912044459576628, 0.02523777754709592702, 0.02574210609834600566, 0.02624643464959608777, 0.02725509175209624851, 0.02826374885459641273, 0.02927240595709657001, 0.03028106305959672728, 0.03128972016209689150, 0.03229837726459704877 ),
 .UNSPECIFIED. ) ;
#1537 =( GEOMETRIC_REPRESENTATION_CONTEXT ( 3 ) GLOBAL_UNCERTAINTY_ASSIGNED_CONTEXT ( ( #2061 ) ) GLOBAL_UNIT_ASSIGNED_CONTEXT ( ( #80, #1589, #1057 ) ) REPRESENTATION_CONTEXT ( 'NONE', 'WORKASPACE' ) );
#1538 = SURFACE_STYLE_FILL_AREA ( #327 ) ;
#1539 = CARTESIAN_POINT ( 'NONE',  ( -2.300000000000000266, -72.60000000000000853, -1.734723475976807094E-15 ) ) ;
#1540 = CARTESIAN_POINT ( 'NONE',  ( 8.324422814932072257, -52.79999999999999716, 2.231815450537910195 ) ) ;
#1541 = VERTEX_POINT ( 'NONE', #3264 ) ;
#1542 = FACE_OUTER_BOUND ( 'NONE', #2880, .T. ) ;
#1543 =( NAMED_UNIT ( * ) PLANE_ANGLE_UNIT ( ) SI_UNIT ( $, .RADIAN. ) );
#1544 = CARTESIAN_POINT ( 'NONE',  ( 6.877134118866902845, -50.00000000000000000, 5.285102517562147995 ) ) ;
#1545 = CARTESIAN_POINT ( 'NONE',  ( -1.654849718955805127, -7.321828482412975347, 4.729586325473386310 ) ) ;
#1546 = ORIENTED_EDGE ( 'NONE', *, *, #1517, .F. ) ;
#1547 = DIRECTION ( 'NONE',  ( -1.000000000000000000, 0.000000000000000000, 0.000000000000000000 ) ) ;
#1548 = SHAPE_DEFINITION_REPRESENTATION ( #3134, #2799 ) ;
#1549 = CARTESIAN_POINT ( 'NONE',  ( 2.250215587473118450, -47.20000000000001705, 8.376503107919017310 ) ) ;
#1550 = CARTESIAN_POINT ( 'NONE',  ( -4.769696007084729850, -50.00000000000000000, 1.499999999999994449 ) ) ;
#1551 = DIRECTION ( 'NONE',  ( 0.000000000000000000, -1.000000000000000000, 0.000000000000000000 ) ) ;
#1552 = DIRECTION ( 'NONE',  ( 0.000000000000000000, 0.9987523388778448696, 0.04993761694388874905 ) ) ;
#1553 = EDGE_CURVE ( 'NONE', #1839, #3036, #634, .T. ) ;
#1554 = CARTESIAN_POINT ( 'NONE',  ( 9.597428871123410588, -51.34559595270280852, 0.3947853968998988328 ) ) ;
#1555 = CARTESIAN_POINT ( 'NONE',  ( -2.250215587473127332, -50.00000000000000000, 8.376503107917878665 ) ) ;
#1556 = ORIENTED_EDGE ( 'NONE', *, *, #909, .T. ) ;
#1557 = CARTESIAN_POINT ( 'NONE',  ( -0.2669266955305334976, -119.1574544647984766, 0.7479247211079949054 ) ) ;
#1558 = DIRECTION ( 'NONE',  ( 0.000000000000000000, 0.000000000000000000, 1.000000000000000000 ) ) ;
#1559 = ORIENTED_EDGE ( 'NONE', *, *, #15, .T. ) ;
#1560 = CARTESIAN_POINT ( 'NONE',  ( 4.782644271597511043, -50.39484142078823226, 1.460283231774381907 ) ) ;
#1561 = CARTESIAN_POINT ( 'NONE',  ( 1.492255338562904265, -47.20000000000001705, 11.39999999999999680 ) ) ;
#1562 = CARTESIAN_POINT ( 'NONE',  ( -4.716912583111715129, -73.70908199638046199, 1.666493794562607933 ) ) ;
#1563 = CARTESIAN_POINT ( 'NONE',  ( 0.000000000000000000, -60.00000000000000000, 0.000000000000000000 ) ) ;
#1564 = VERTEX_POINT ( 'NONE', #295 ) ;
#1565 = PRESENTATION_STYLE_ASSIGNMENT (( #2332 ) ) ;
#1566 = VECTOR ( 'NONE', #2425, 1000.000000000000000 ) ;
#1567 = DIRECTION ( 'NONE',  ( -0.000000000000000000, -0.000000000000000000, 1.000000000000000000 ) ) ;
#1568 = CARTESIAN_POINT ( 'NONE',  ( -8.160064090060583197, -50.00000000000000000, 2.773119917861301964 ) ) ;
#1569 = VERTEX_POINT ( 'NONE', #2070 ) ;
#1570 = B_SPLINE_CURVE_WITH_KNOTS ( 'NONE', 3,
 ( #379, #1103, #2939, #2433, #1665, #2908, #159, #1138, #345, #681, #1352, #1683 ),
 .UNSPECIFIED., .F., .F.,
 ( 4, 2, 2, 2, 2, 4 ),
 ( 0.002704438958034565722, 0.003382491784585806537, 0.004060544611137047351, 0.004738597437688288165, 0.005077623850963906837, 0.005416650264239525510 ),
 .UNSPECIFIED. ) ;
#1571 = CARTESIAN_POINT ( 'NONE',  ( 5.000000000000000000, 5.590169943749473624, 18.00000000000000355 ) ) ;
#1572 = VECTOR ( 'NONE', #1841, 1000.000000000000000 ) ;
#1573 = ADVANCED_FACE ( 'NONE', ( #515, #1542 ), #1767, .T. ) ;
#1574 = CARTESIAN_POINT ( 'NONE',  ( 2.250215587473118450, -50.00000000000000000, 8.376503107919017310 ) ) ;
#1575 = CARTESIAN_POINT ( 'NONE',  ( 0.000000000000000000, -72.50000000000001421, -2.500000000000000444 ) ) ;
#1576 = EDGE_LOOP ( 'NONE', ( #2037, #1632, #2864, #260, #1799, #1604 ) ) ;
#1577 = CARTESIAN_POINT ( 'NONE',  ( 0.8424979979451828749, 7.454395415945072045, -4.931395878866434046 ) ) ;
#1578 = CARTESIAN_POINT ( 'NONE',  ( 11.03470001049147697, -47.20000000000001705, 2.958453039086267111 ) ) ;
#1579 = ORIENTED_EDGE ( 'NONE', *, *, #273, .T. ) ;
#1580 = CARTESIAN_POINT ( 'NONE',  ( -4.987611521976591078, -51.45995144009268074, -0.3958319429405975920 ) ) ;
#1581 = VECTOR ( 'NONE', #920, 1000.000000000000000 ) ;
#1582 = DIRECTION ( 'NONE',  ( -0.000000000000000000, -0.000000000000000000, -1.000000000000000000 ) ) ;
#1583 = VERTEX_POINT ( 'NONE', #2288 ) ;
#1584 = CARTESIAN_POINT ( 'NONE',  ( 0.000000000000000000, 0.000000000000000000, -10.00000000000000000 ) ) ;
#1585 = CARTESIAN_POINT ( 'NONE',  ( 5.285102517541700351, -50.00000000000000000, 6.877134118846478295 ) ) ;
#1586 =( GEOMETRIC_REPRESENTATION_CONTEXT ( 3 ) GLOBAL_UNCERTAINTY_ASSIGNED_CONTEXT ( ( #3019 ) ) GLOBAL_UNIT_ASSIGNED_CONTEXT ( ( #2071, #828, #3058 ) ) REPRESENTATION_CONTEXT ( 'NONE', 'WORKASPACE' ) );
#1587 = ORIENTED_EDGE ( 'NONE', *, *, #2588, .F. ) ;
#1588 = DIRECTION ( 'NONE',  ( 1.000000000000000000, 0.000000000000000000, 0.000000000000000000 ) ) ;
#1589 =( NAMED_UNIT ( * ) PLANE_ANGLE_UNIT ( ) SI_UNIT ( $, .RADIAN. ) );
#1590 = CARTESIAN_POINT ( 'NONE',  ( 5.000292928619530564, 5.589907940605836956, -0.3348667354298545673 ) ) ;
#1591 = CARTESIAN_POINT ( 'NONE',  ( -2.312079649032890760, -64.45380699776846711, 4.445949067509105568 ) ) ;
#1592 = CARTESIAN_POINT ( 'NONE',  ( -3.078112602769041306, -6.845324219060942461, 3.953457562721318652 ) ) ;
#1593 = EDGE_LOOP ( 'NONE', ( #1526, #949, #2318, #1200 ) ) ;
#1594 = CARTESIAN_POINT ( 'NONE',  ( -3.078327448814686562, 6.845130131842670274, -3.953084837412474517 ) ) ;
#1595 = MANIFOLD_SOLID_BREP ( 'AdvancedHole1', #2472 ) ;
#1596 = CARTESIAN_POINT ( 'NONE',  ( -8.599999999999996092, -47.20000000000001705, -1.366666666666159546 ) ) ;
#1597 = ORIENTED_EDGE ( 'NONE', *, *, #755, .T. ) ;
#1598 = CARTESIAN_POINT ( 'NONE',  ( -1.532095834638425913, -71.98215106548155973, -4.761538506183794262 ) ) ;
#1599 = CARTESIAN_POINT ( 'NONE',  ( -6.877134118866000456, -50.00000000000000000, 5.285102517561346858 ) ) ;
#1600 = ORIENTED_EDGE ( 'NONE', *, *, #672, .T. ) ;
#1601 = CARTESIAN_POINT ( 'NONE',  ( 3.950486495955891025E-15, -119.2999999999982776, 0.7850000000000663114 ) ) ;
#1602 = LINE ( 'NONE', #823, #732 ) ;
#1603 = CARTESIAN_POINT ( 'NONE',  ( -6.877134118866001344, -52.79999999999999716, 5.285102517561345969 ) ) ;
#1604 = ORIENTED_EDGE ( 'NONE', *, *, #1115, .F. ) ;
#1605 = CYLINDRICAL_SURFACE ( 'NONE', #740, 6.000000000000001776 ) ;
#1606 = SURFACE_SIDE_STYLE ('',( #2603 ) ) ;
#1607 = CARTESIAN_POINT ( 'NONE',  ( 3.320792018548207825, 6.729571896343306214, -3.751470290485135806 ) ) ;
#1608 = LINE ( 'NONE', #2624, #585 ) ;
#1609 = CARTESIAN_POINT ( 'NONE',  ( -11.36325033731746004, -50.00000000000000000, 0.9334869871344717573 ) ) ;
#1610 = ORIENTED_EDGE ( 'NONE', *, *, #2781, .F. ) ;
#1611 = CARTESIAN_POINT ( 'NONE',  ( 9.999999999999976907, -48.60000000000000142, -1.084199742356775455E-20 ) ) ;
#1612 = MANIFOLD_SOLID_BREP ( 'Sweep1', #141 ) ;
#1613 = CARTESIAN_POINT ( 'NONE',  ( -11.36325033731746004, -50.00000000000000000, 0.9334869871344717573 ) ) ;
#1614 = EDGE_LOOP ( 'NONE', ( #2024, #2244, #3174, #3066, #2457 ) ) ;
#1615 = CARTESIAN_POINT ( 'NONE',  ( -9.999999999999998224, -48.60000000000000142, 1.734719587726169024E-19 ) ) ;
#1616 = DIRECTION ( 'NONE',  ( -0.000000000000000000, -0.000000000000000000, 1.000000000000000000 ) ) ;
#1617 = ORIENTED_EDGE ( 'NONE', *, *, #104, .T. ) ;
#1618 = SURFACE_STYLE_FILL_AREA ( #410 ) ;
#1619 = CARTESIAN_POINT ( 'NONE',  ( 11.64000000000000057, -50.00000000000000000, -1.399999999999999911 ) ) ;
#1620 = LINE ( 'NONE', #1652, #1581 ) ;
#1621 = VERTEX_POINT ( 'NONE', #16 ) ;
#1622=STYLED_ITEM('',(#3293),#1612);
#1623 = DIRECTION ( 'NONE',  ( -0.000000000000000000, -0.000000000000000000, -1.000000000000000000 ) ) ;
#1624 = LINE ( 'NONE', #2623, #1511 ) ;
#1625 = CARTESIAN_POINT ( 'NONE',  ( -11.37702123033536061, -47.20000000000001705, 0.7471912688805021352 ) ) ;
#1626 = PRODUCT ( 'Needle', 'Needle', '', ( #3080 ) ) ;
#1627 = EDGE_LOOP ( 'NONE', ( #373, #3027 ) ) ;
#1628 = CARTESIAN_POINT ( 'NONE',  ( -0.1683266833682984520, 7.500000000000003553, -5.000000000000000000 ) ) ;
#1629 = CARTESIAN_POINT ( 'NONE',  ( 11.39539595717853082, -50.00000000000000000, 0.3739757293042009212 ) ) ;
#1630 = VERTEX_POINT ( 'NONE', #1021 ) ;
#1631 = DIRECTION ( 'NONE',  ( 0.000000000000000000, 1.000000000000000000, 0.000000000000000000 ) ) ;
#1632 = ORIENTED_EDGE ( 'NONE', *, *, #2617, .T. ) ;
#1633 = CYLINDRICAL_SURFACE ( 'NONE', #2702, 2.499999999999999556 ) ;
#1634 = LINE ( 'NONE', #344, #980 ) ;
#1635 = FACE_OUTER_BOUND ( 'NONE', #1674, .T. ) ;
#1636 = APPLICATION_CONTEXT ( 'automotive_design' ) ;
#1637 = ORIENTED_EDGE ( 'NONE', *, *, #2448, .T. ) ;
#1638 = DIRECTION ( 'NONE',  ( 0.000000000000000000, 0.9987523388778448696, 0.04993761694388874905 ) ) ;
#1639 = CIRCLE ( 'NONE', #314, 7.500000000000000888 ) ;
#1640 = CARTESIAN_POINT ( 'NONE',  ( -5.742338339643776379, -47.20000000000001705, 9.960716663318299524 ) ) ;
#1641 = CARTESIAN_POINT ( 'NONE',  ( -0.1685493663350521309, -7.499999999999996447, -4.999999999999998224 ) ) ;
#1642 = CARTESIAN_POINT ( 'NONE',  ( -1.658007454526697177, 7.321065759480116952, 4.728400501374060205 ) ) ;
#1643 = EDGE_CURVE ( 'NONE', #1569, #3146, #829, .T. ) ;
#1644 = CARTESIAN_POINT ( 'NONE',  ( 11.39999532361432522, -50.00000000000000000, 0.1755699507458462760 ) ) ;
#1645 = STYLED_ITEM ( 'NONE', ( #1565 ), #617 ) ;
#1646 = ORIENTED_EDGE ( 'NONE', *, *, #986, .T. ) ;
#1647 = CARTESIAN_POINT ( 'NONE',  ( -2.499999999999990230, -70.16572065136264769, -4.330127018922198090 ) ) ;
#1648 = PRODUCT_DEFINITION ( 'UNKNOWN', '', #1849, #506 ) ;
#1649 = ORIENTED_EDGE ( 'NONE', *, *, #1789, .T. ) ;
#1650 = PRODUCT_DEFINITION_SHAPE ( 'NONE', 'NONE',  #3276 ) ;
#1651 = CARTESIAN_POINT ( 'NONE',  ( 8.489369361306732031, -50.00000000000000000, 1.403517616196621409 ) ) ;
#1652 = CARTESIAN_POINT ( 'NONE',  ( 7.500000000000000000, 9.184850993605147944E-16, 10.00000000000000000 ) ) ;
#1653 = ORIENTED_EDGE ( 'NONE', *, *, #2059, .F. ) ;
#1654 = FACE_OUTER_BOUND ( 'NONE', #1371, .T. ) ;
#1655 = CARTESIAN_POINT ( 'NONE',  ( 11.30825875096014066, -47.20000000000001705, 1.490875164968454625 ) ) ;
#1656 = CARTESIAN_POINT ( 'NONE',  ( -10.81682914263834405, -50.00000000000000000, 3.675996170188739143 ) ) ;
#1657 = CARTESIAN_POINT ( 'NONE',  ( 0.2999999999999837796, -118.9999999999982379, 0.7416198487096254954 ) ) ;
#1658 = CARTESIAN_POINT ( 'NONE',  ( 11.39999999999999680, -50.00000000000000000, -1.639999999999997460 ) ) ;
#1659 = ORIENTED_EDGE ( 'NONE', *, *, #1771, .T. ) ;
#1660 = CARTESIAN_POINT ( 'NONE',  ( -8.904708611508519667, -49.04279439154561970, 1.036389030864862448 ) ) ;
#1661 = CYLINDRICAL_SURFACE ( 'NONE', #1481, 2.500000000000000444 ) ;
#1662 = ORIENTED_EDGE ( 'NONE', *, *, #1043, .T. ) ;
#1663 = CYLINDRICAL_SURFACE ( 'NONE', #947, 4.999999999999999112 ) ;
#1664 = CARTESIAN_POINT ( 'NONE',  ( 8.600005876649037262, -50.00000000000000000, -0.2541998246239300374 ) ) ;
#1665 = CARTESIAN_POINT ( 'NONE',  ( 8.904708611508466376, -49.04279439154559128, 1.036389030864799832 ) ) ;
#1666 = ORIENTED_EDGE ( 'NONE', *, *, #1483, .T. ) ;
#1667 = CARTESIAN_POINT ( 'NONE',  ( -4.769696007084729850, -50.00000000000000000, 1.499999999999994449 ) ) ;
#1668 = CARTESIAN_POINT ( 'NONE',  ( -7.005833569763921354, -47.20000000000001705, 9.116201041262108618 ) ) ;
#1669 =( NAMED_UNIT ( * ) PLANE_ANGLE_UNIT ( ) SI_UNIT ( $, .RADIAN. ) );
#1670 = CARTESIAN_POINT ( 'NONE',  ( -8.485280282859317680, -50.00000000000000000, 1.400000000000003020 ) ) ;
#1671 = AXIS2_PLACEMENT_3D ( 'NONE', #883, #121, #897 ) ;
#1672 = CARTESIAN_POINT ( 'NONE',  ( -11.39999999999999680, -50.00000000000000000, -1.366666666666159768 ) ) ;
#1673 = CIRCLE ( 'NONE', #3159, 7.500000000000000000 ) ;
#1674 = EDGE_LOOP ( 'NONE', ( #1706, #2788 ) ) ;
#1675 = CARTESIAN_POINT ( 'NONE',  ( 8.582665138674004268, -47.20000000000001705, 0.5636706063485154017 ) ) ;
#1676 = DIRECTION ( 'NONE',  ( 0.000000000000000000, -1.000000000000000000, 0.000000000000000000 ) ) ;
#1677 = EDGE_CURVE ( 'NONE', #1911, #2713, #2948, .T. ) ;
#1678 = CIRCLE ( 'NONE', #1729, 6.000000000000001776 ) ;
#1679 = CARTESIAN_POINT ( 'NONE',  ( 0.000000000000000000, -60.00000000000000000, 0.000000000000000000 ) ) ;
#1680 = ORIENTED_EDGE ( 'NONE', *, *, #2510, .F. ) ;
#1681 = CARTESIAN_POINT ( 'NONE',  ( 1.696011499264681532, -64.23548717087807347, 4.715485471644023541 ) ) ;
#1682 = CARTESIAN_POINT ( 'NONE',  ( -8.599999999999996092, -47.20000000000001705, -1.639999999999997460 ) ) ;
#1683 = CARTESIAN_POINT ( 'NONE',  ( 9.999999999999976907, -48.60000000000000142, -1.084199742356775455E-20 ) ) ;
#1684 = CARTESIAN_POINT ( 'NONE',  ( 10.97094949647942030, -51.01251636945240620, -0.9709494964794326277 ) ) ;
#1685 = DIRECTION ( 'NONE',  ( -0.000000000000000000, -0.000000000000000000, -1.000000000000000000 ) ) ;
#1686 = CARTESIAN_POINT ( 'NONE',  ( -11.40000778997679198, -47.20000000000001705, -0.2924664341913127408 ) ) ;
#1687 = AXIS2_PLACEMENT_3D ( 'NONE', #771, #1775, #1794 ) ;
#1688 = CARTESIAN_POINT ( 'NONE',  ( -0.07895800510998150779, -114.6999999999982975, 1.014999999999999902 ) ) ;
#1689 = DIRECTION ( 'NONE',  ( 1.000000000000000000, 0.000000000000000000, 0.000000000000000000 ) ) ;
#1690 = AXIS2_PLACEMENT_3D ( 'NONE', #1984, #2956, #445 ) ;
#1691 = CARTESIAN_POINT ( 'NONE',  ( 2.250215587473118450, -52.79999999999999716, 8.376503107919017310 ) ) ;
#1692 = AXIS2_PLACEMENT_3D ( 'NONE', #3075, #2051, #2104 ) ;
#1693 = ORIENTED_EDGE ( 'NONE', *, *, #1928, .T. ) ;
#1694 = CARTESIAN_POINT ( 'NONE',  ( 8.572276570257084671, -50.00000000000000000, 0.7042094815225934390 ) ) ;
#1695 = CARTESIAN_POINT ( 'NONE',  ( 11.03726195774814833, -49.04331167652343026, -1.037261957748134344 ) ) ;
#1696 = VERTEX_POINT ( 'NONE', #381 ) ;
#1697 = CARTESIAN_POINT ( 'NONE',  ( 0.8675805444301170066, -64.06058600797459235, 4.927173720332874041 ) ) ;
#1698 = LINE ( 'NONE', #935, #2155 ) ;
#1699 = DIRECTION ( 'NONE',  ( 0.000000000000000000, 1.000000000000000000, 0.000000000000000000 ) ) ;
#1700 = PLANE ( 'NONE',  #1998 ) ;
#1701 = FACE_OUTER_BOUND ( 'NONE', #389, .T. ) ;
#1702 = CARTESIAN_POINT ( 'NONE',  ( 11.37702123033542279, -50.00000000000000000, 0.7471912688806704450 ) ) ;
#1703 = CARTESIAN_POINT ( 'NONE',  ( 2.500000000000008438, -70.00000000000000000, 10.00000000000000000 ) ) ;
#1704 = CARTESIAN_POINT ( 'NONE',  ( -8.485280282859321233, -50.11569792258599421, 1.400000000000003242 ) ) ;
#1705 = CARTESIAN_POINT ( 'NONE',  ( 8.572276570257082895, -52.79999999999999716, 0.7042094815225934390 ) ) ;
#1706 = ORIENTED_EDGE ( 'NONE', *, *, #2414, .F. ) ;
#1707 = CARTESIAN_POINT ( 'NONE',  ( 8.489369361306732031, -50.00000000000000000, 1.403517616196621409 ) ) ;
#1708 = DIRECTION ( 'NONE',  ( 0.000000000000000000, 0.000000000000000000, -1.000000000000000000 ) ) ;
#1709 = CARTESIAN_POINT ( 'NONE',  ( 0.6741883319902871596, -7.471549563736964217, -4.957238835368188212 ) ) ;
#1710 = ORIENTED_EDGE ( 'NONE', *, *, #2762, .F. ) ;
#1711 = CARTESIAN_POINT ( 'NONE',  ( 3.790413940515792390, -65.34115326502070786, 3.275345238443577944 ) ) ;
#1712 = EDGE_CURVE ( 'NONE', #3153, #277, #569, .T. ) ;
#1713 = CARTESIAN_POINT ( 'NONE',  ( -8.582665138674013150, -50.00000000000000000, 0.5636706063486749407 ) ) ;
#1714 = LINE ( 'NONE', #1003, #898 ) ;
#1715 = ADVANCED_FACE ( 'NONE', ( #1355 ), #866, .T. ) ;
#1716 = ORIENTED_EDGE ( 'NONE', *, *, #2762, .T. ) ;
#1717 = CARTESIAN_POINT ( 'NONE',  ( 0.000000000000000000, -67.40000000000000568, 0.000000000000000000 ) ) ;
#1718 = EDGE_CURVE ( 'NONE', #1630, #1979, #2277, .T. ) ;
#1719 = CARTESIAN_POINT ( 'NONE',  ( 9.959683570760574867, -50.00000000000000000, 5.743837162466680191 ) ) ;
#1720 = CARTESIAN_POINT ( 'NONE',  ( 10.81682914263883610, -50.00000000000000000, 3.675996170187548540 ) ) ;
#1721 = DIRECTION ( 'NONE',  ( 1.000000000000000000, -0.000000000000000000, 0.000000000000000000 ) ) ;
#1722 = CARTESIAN_POINT ( 'NONE',  ( 8.599999999999996092, -52.79999999999999716, -1.366666666666861873 ) ) ;
#1723 = ORIENTED_EDGE ( 'NONE', *, *, #1153, .F. ) ;
#1724 = CARTESIAN_POINT ( 'NONE',  ( -5.285102517542626721, -47.20000000000001705, 6.877134118847253674 ) ) ;
#1725 = CIRCLE ( 'NONE', #296, 2.499999999999999556 ) ;
#1726 = CYLINDRICAL_SURFACE ( 'NONE', #2593, 7.500000000000000000 ) ;
#1727 = DIRECTION ( 'NONE',  ( 0.000000000000000000, 0.000000000000000000, 1.000000000000000000 ) ) ;
#1728 = CARTESIAN_POINT ( 'NONE',  ( 4.475554532957461085, -65.99917996832718359, 2.251442214368883477 ) ) ;
#1729 = AXIS2_PLACEMENT_3D ( 'NONE', #240, #1504, #2528 ) ;
#1730 = CARTESIAN_POINT ( 'NONE',  ( 6.877134118866901957, -47.20000000000001705, 5.285102517562147995 ) ) ;
#1731 = DIRECTION ( 'NONE',  ( 1.000000000000000000, 0.000000000000000000, -0.000000000000000000 ) ) ;
#1732 = ORIENTED_EDGE ( 'NONE', *, *, #59, .T. ) ;
#1733 = ADVANCED_FACE ( 'NONE', ( #2653 ), #2369, .T. ) ;
#1734 = CARTESIAN_POINT ( 'NONE',  ( -8.599999999999996092, -50.00000000000000000, -1.639999999999997460 ) ) ;
#1735 = CARTESIAN_POINT ( 'NONE',  ( 11.30825875096042310, -52.79999999999999716, 1.490875164968454625 ) ) ;
#1736 = CARTESIAN_POINT ( 'NONE',  ( 11.40000778997679021, -50.00000000000000000, -0.2924664341912772692 ) ) ;
#1737 = CARTESIAN_POINT ( 'NONE',  ( -11.33527052789730405, -50.43454227690136094, -1.335270527897301385 ) ) ;
#1738 = B_SPLINE_CURVE_WITH_KNOTS ( 'NONE', 3,
 ( #369, #3135, #1393, #2143, #869, #164, #3150, #3197, #1609, #2655, #3167, #2914, #1656, #2669, #399, #1408, #2944, #436, #2007, #3262, #1976, #1239, #1225, #2979, #1493, #1720, #750, #484, #2994, #973, #1254, #686, #992, #1736, #940, #451, #1455, #2489 ),
 .UNSPECIFIED., .F., .F.,
 ( 4, 2, 2, 2, 2, 2, 2, 2, 2, 2, 2, 2, 2, 2, 2, 2, 2, 2, 4 ),
 ( -0.04443856763921243819, -0.02602830390294905150, 0.000000000000000000, 0.01562500000000000694, 0.03125000000000000694, 0.06250000000000000000, 0.1250000000000000000, 0.2500000000000000000, 0.3750000000000000000, 0.4999999999999999445, 0.6250000000000000000, 0.7500000000000000000, 0.8750000000000000000, 0.9374999999999998890, 0.9687500000000001110, 0.9843750000000001110, 1.000000000000000000, 1.026028303902949190, 1.044438567639293325 ),
 .UNSPECIFIED. ) ;
#1739 = ADVANCED_FACE ( 'NONE', ( #2405 ), #1337, .F. ) ;
#1740 = CIRCLE ( 'NONE', #106, 2.500000000000000000 ) ;
#1741 = CARTESIAN_POINT ( 'NONE',  ( -8.160064090060583197, -52.79999999999999716, 2.773119917861301520 ) ) ;
#1742 = ORIENTED_EDGE ( 'NONE', *, *, #2081, .F. ) ;
#1743 = AXIS2_PLACEMENT_3D ( 'NONE', #331, #2351, #1832 ) ;
#1744 = CARTESIAN_POINT ( 'NONE',  ( 1.125736483476999839, -50.00000000000000000, 8.599999999999996092 ) ) ;
#1745 = CARTESIAN_POINT ( 'NONE',  ( 0.3416648584763157803, -7.500000000000000888, 5.000000000000000888 ) ) ;
#1746 = FACE_OUTER_BOUND ( 'NONE', #1121, .T. ) ;
#1747 = CARTESIAN_POINT ( 'NONE',  ( -10.61784491273703246, -48.73341048396267894, -0.6178437967800078923 ) ) ;
#1748 = VERTEX_POINT ( 'NONE', #1389 ) ;
#1749 = DIRECTION ( 'NONE',  ( 0.000000000000000000, 0.000000000000000000, -1.000000000000000000 ) ) ;
#1750 = CARTESIAN_POINT ( 'NONE',  ( -8.599999999999996092, -52.79999999999999716, -1.639999999999997460 ) ) ;
#1751 = CARTESIAN_POINT ( 'NONE',  ( 4.856127559802944305, -49.08436397556629061, -1.192133730937313008 ) ) ;
#1752 = CARTESIAN_POINT ( 'NONE',  ( 2.348910296171192290E-13, -114.6999999999962228, -1.015000000000727765 ) ) ;
#1753 = CARTESIAN_POINT ( 'NONE',  ( -2.250215587473127332, -52.79999999999999716, 8.376503107917878665 ) ) ;
#1754 = VERTEX_POINT ( 'NONE', #1089 ) ;
#1755 = CARTESIAN_POINT ( 'NONE',  ( 2.348910296171192290E-13, -114.6999999999962228, -1.015000000000727765 ) ) ;
#1756 = CONTEXT_DEPENDENT_SHAPE_REPRESENTATION ( #2211, #1148 ) ;
#1757 = FACE_OUTER_BOUND ( 'NONE', #673, .T. ) ;
#1758 = EDGE_CURVE ( 'NONE', #1093, #129, #3131, .T. ) ;
#1759 = EDGE_CURVE ( 'NONE', #2825, #1786, #2488, .T. ) ;
#1760 = DIRECTION ( 'NONE',  ( -0.000000000000000000, -0.000000000000000000, 1.000000000000000000 ) ) ;
#1761 = UNCERTAINTY_MEASURE_WITH_UNIT (LENGTH_MEASURE( 1.000000000000000082E-05 ), #2666, 'distance_accuracy_value', 'NONE');
#1762 = CYLINDRICAL_SURFACE ( 'NONE', #2539, 2.499999999999999556 ) ;
#1763 = DIRECTION ( 'NONE',  ( 1.000000000000000000, 0.000000000000000000, 0.000000000000000000 ) ) ;
#1764 = DIRECTION ( 'NONE',  ( 0.000000000000000000, -1.000000000000000000, -0.000000000000000000 ) ) ;
#1765 = CARTESIAN_POINT ( 'NONE',  ( -8.599999999999996092, -52.79999999999999716, -1.366666666666159546 ) ) ;
#1766 = ORIENTED_EDGE ( 'NONE', *, *, #2947, .T. ) ;
#1767 = CYLINDRICAL_SURFACE ( 'NONE', #2830, 7.500000000000000000 ) ;
#1768 = CARTESIAN_POINT ( 'NONE',  ( -4.331939449206426929, -50.00000000000000000, 7.514224851276241957 ) ) ;
#1769 = ORIENTED_EDGE ( 'NONE', *, *, #2712, .T. ) ;
#1770 = CARTESIAN_POINT ( 'NONE',  ( 1.654328459400600471, 7.322002074975777930, -4.729864656991090932 ) ) ;
#1771 = EDGE_CURVE ( 'NONE', #2794, #1333, #348, .T. ) ;
#1772 = CARTESIAN_POINT ( 'NONE',  ( -4.724063086364457931, -66.29587799920766145, 1.668329630282862963 ) ) ;
#1773 = CIRCLE ( 'NONE', #2885, 7.500000000000000000 ) ;
#1774 = CARTESIAN_POINT ( 'NONE',  ( -4.769696007084725409, -50.09973230823852219, -1.500000000000006661 ) ) ;
#1775 = DIRECTION ( 'NONE',  ( 0.000000000000000000, 1.000000000000000000, 0.000000000000000000 ) ) ;
#1776 = DIRECTION ( 'NONE',  ( -1.000000000000000000, 0.000000000000000000, 0.000000000000000000 ) ) ;
#1777 = APPLICATION_PROTOCOL_DEFINITION ( 'draft international standard', 'automotive_design', 1998, #1345 ) ;
#1778 = EDGE_CURVE ( 'NONE', #842, #216, #690, .T. ) ;
#1779 = FACE_BOUND ( 'NONE', #500, .T. ) ;
#1780 = CARTESIAN_POINT ( 'NONE',  ( 4.331939449206418047, -52.79999999999999716, 7.514224851275111305 ) ) ;
#1781 = ORIENTED_EDGE ( 'NONE', *, *, #401, .F. ) ;
#1782 = DIRECTION ( 'NONE',  ( 0.000000000000000000, 1.000000000000000000, 0.000000000000000000 ) ) ;
#1783 = CARTESIAN_POINT ( 'NONE',  ( 2.500000000000008438, -70.00000000000000000, -4.330127018922187432 ) ) ;
#1784 = CARTESIAN_POINT ( 'NONE',  ( -5.285102517542626721, -50.00000000000000000, 6.877134118847252786 ) ) ;
#1785 = CARTESIAN_POINT ( 'NONE',  ( 7.500000000000000888, 30.00000000000000000, 18.00000000000000355 ) ) ;
#1786 = VERTEX_POINT ( 'NONE', #1140 ) ;
#1787 = CARTESIAN_POINT ( 'NONE',  ( 4.769696007084725409, -50.09970496801165751, -1.500000000000006217 ) ) ;
#1788 = CARTESIAN_POINT ( 'NONE',  ( -8.489369361306263073, -47.20000000000001705, 1.403517616197273554 ) ) ;
#1789 = EDGE_CURVE ( 'NONE', #2919, #2109, #2645, .T. ) ;
#1790 = CIRCLE ( 'NONE', #371, 7.500000000000000888 ) ;
#1791 = CARTESIAN_POINT ( 'NONE',  ( -0.8675805444301208924, -75.93941399202543607, 4.927173720332874041 ) ) ;
#1792 = UNCERTAINTY_MEASURE_WITH_UNIT (LENGTH_MEASURE( 1.000000000000000082E-05 ), #1945, 'distance_accuracy_value', 'NONE');
#1793 = CIRCLE ( 'NONE', #1690, 7.500000000000000888 ) ;
#1794 = DIRECTION ( 'NONE',  ( 0.000000000000000000, 0.000000000000000000, 1.000000000000000000 ) ) ;
#1795 = CYLINDRICAL_SURFACE ( 'NONE', #2780, 7.500000000000000000 ) ;
#1796 =( NAMED_UNIT ( * ) PLANE_ANGLE_UNIT ( ) SI_UNIT ( $, .RADIAN. ) );
#1797 = CARTESIAN_POINT ( 'NONE',  ( 5.000000000000000000, 30.00000000000000000, -21.62277660168378901 ) ) ;
#1798 = CARTESIAN_POINT ( 'NONE',  ( -8.572276570256935457, -50.00000000000000000, 0.7042094815226510596 ) ) ;
#1799 = ORIENTED_EDGE ( 'NONE', *, *, #2087, .F. ) ;
#1800 = CARTESIAN_POINT ( 'NONE',  ( 0.07895800510998153554, -114.6999999999983402, -1.014999999999999902 ) ) ;
#1801 = CARTESIAN_POINT ( 'NONE',  ( 8.572276570257084671, -50.00000000000000000, 0.7042094815225934390 ) ) ;
#1802 = DIRECTION ( 'NONE',  ( 0.000000000000000000, 1.000000000000000000, 0.000000000000000000 ) ) ;
#1803 = ORIENTED_EDGE ( 'NONE', *, *, #347, .T. ) ;
#1804 = CARTESIAN_POINT ( 'NONE',  ( -0.2671601197814520434, -114.8429732948149535, -0.9734511544928146076 ) ) ;
#1805 = APPLICATION_PROTOCOL_DEFINITION ( 'draft international standard', 'automotive_design', 1998, #3220 ) ;
#1806 = CARTESIAN_POINT ( 'NONE',  ( -11.39539595717859299, -47.20000000000001705, 0.3739757293043587949 ) ) ;
#1807 = EDGE_LOOP ( 'NONE', ( #1579, #1464, #20, #3186, #360, #2681 ) ) ;
#1808 = CARTESIAN_POINT ( 'NONE',  ( -4.997016223860688555, -51.49013799948261294, 0.1978941090189494934 ) ) ;
#1809 = DIRECTION ( 'NONE',  ( -0.000000000000000000, 1.000000000000000000, -0.000000000000000000 ) ) ;
#1810 = VERTEX_POINT ( 'NONE', #847 ) ;
#1811 =( NAMED_UNIT ( * ) SI_UNIT ( $, .STERADIAN. ) SOLID_ANGLE_UNIT ( ) );
#1812 = FACE_BOUND ( 'NONE', #312, .T. ) ;
#1813 = CARTESIAN_POINT ( 'NONE',  ( -1.125736483477000061, -52.79999999999999716, 8.599999999999996092 ) ) ;
#1814 = ORIENTED_EDGE ( 'NONE', *, *, #2657, .T. ) ;
#1815 = DIRECTION ( 'NONE',  ( -0.000000000000000000, -0.000000000000000000, -1.000000000000000000 ) ) ;
#1816 = EDGE_CURVE ( 'NONE', #38, #2923, #3164, .T. ) ;
#1817 = CARTESIAN_POINT ( 'NONE',  ( -2.250215587473127332, -50.00000000000000000, 8.376503107917878665 ) ) ;
#1818 = CARTESIAN_POINT ( 'NONE',  ( 8.469856736028367195, -50.00000000000000000, 1.493482969799619031 ) ) ;
#1819 = ORIENTED_EDGE ( 'NONE', *, *, #811, .T. ) ;
#1820 = CARTESIAN_POINT ( 'NONE',  ( -0.07907397510870849133, -114.6999999999981412, -1.015000000000068514 ) ) ;
#1821 = ADVANCED_FACE ( 'NONE', ( #2860 ), #1605, .T. ) ;
#1822 = CARTESIAN_POINT ( 'NONE',  ( -8.160064090060583197, -47.20000000000001705, 2.773119917861301520 ) ) ;
#1823 = ORIENTED_EDGE ( 'NONE', *, *, #2062, .T. ) ;
#1824 = CARTESIAN_POINT ( 'NONE',  ( -4.784663389310397363, -50.39016944930146735, -1.451689076663209566 ) ) ;
#1825 = AXIS2_PLACEMENT_3D ( 'NONE', #1525, #783, #588 ) ;
#1826 = CYLINDRICAL_SURFACE ( 'NONE', #2942, 0.2999999999999999889 ) ;
#1827 = ORIENTED_EDGE ( 'NONE', *, *, #2234, .T. ) ;
#1828 = AXIS2_PLACEMENT_3D ( 'NONE', #469, #670, #1689 ) ;
#1829 = LINE ( 'NONE', #2634, #3099 ) ;
#1830 = CARTESIAN_POINT ( 'NONE',  ( -1.125736483476999839, -50.00000000000000000, 8.599999999999996092 ) ) ;
#1831 = ORIENTED_EDGE ( 'NONE', *, *, #2507, .T. ) ;
#1832 = DIRECTION ( 'NONE',  ( 0.000000000000000000, 0.000000000000000000, -1.000000000000000000 ) ) ;
#1833 = CARTESIAN_POINT ( 'NONE',  ( -1.464466094067260249, -67.50000000000000000, -2.499999999999996447 ) ) ;
#1834 = CARTESIAN_POINT ( 'NONE',  ( 3.966867482980610315, -6.368676471623262003, 3.060450018115215443 ) ) ;
#1835 = DIRECTION ( 'NONE',  ( 0.000000000000000000, 0.000000000000000000, 1.000000000000000000 ) ) ;
#1836 = EDGE_LOOP ( 'NONE', ( #203, #2891, #556, #860, #1418, #996 ) ) ;
#1837 = CARTESIAN_POINT ( 'NONE',  ( -4.965855707945498132, 5.621220898751191797, -0.6727113530297602617 ) ) ;
#1838 = CARTESIAN_POINT ( 'NONE',  ( -8.324422814933019055, -47.20000000000001705, 2.231815450536601020 ) ) ;
#1839 = VERTEX_POINT ( 'NONE', #2821 ) ;
#1840 = CARTESIAN_POINT ( 'NONE',  ( -1.263489017627365207, -72.16329285933299786, -4.839748143728395569 ) ) ;
#1841 = DIRECTION ( 'NONE',  ( -0.000000000000000000, -0.000000000000000000, -1.000000000000000000 ) ) ;
#1842 = ORIENTED_EDGE ( 'NONE', *, *, #1029, .F. ) ;
#1843 = FACE_BOUND ( 'NONE', #29, .T. ) ;
#1844 = CARTESIAN_POINT ( 'NONE',  ( 0.000000000000000000, -60.00000000000000000, 0.000000000000000000 ) ) ;
#1845 = CARTESIAN_POINT ( 'NONE',  ( -7.513445500749801553, -52.79999999999999716, 4.333070140105379942 ) ) ;
#1846 = ORIENTED_EDGE ( 'NONE', *, *, #1396, .T. ) ;
#1847 = DIRECTION ( 'NONE',  ( -0.000000000000000000, 1.000000000000000000, -0.000000000000000000 ) ) ;
#1848 = FILL_AREA_STYLE_COLOUR ( '', #950 ) ;
#1849 = PRODUCT_DEFINITION_FORMATION_WITH_SPECIFIED_SOURCE ( 'ANY', '', #2159, .NOT_KNOWN. ) ;
#1850 = CARTESIAN_POINT ( 'NONE',  ( 4.325873777034227707, 6.130418473463322471, -2.527359400829327196 ) ) ;
#1851 = DIRECTION ( 'NONE',  ( -0.000000000000000000, -0.000000000000000000, 1.000000000000000000 ) ) ;
#1852 = LINE ( 'NONE', #814, #466 ) ;
#1853 = VERTEX_POINT ( 'NONE', #1571 ) ;
#1854 = DIRECTION ( 'NONE',  ( -0.000000000000000000, -0.000000000000000000, 1.000000000000000000 ) ) ;
#1855 = CARTESIAN_POINT ( 'NONE',  ( 2.982843918280273510, -50.00000000000000000, 11.10373667793903252 ) ) ;
#1856 = ORIENTED_EDGE ( 'NONE', *, *, #1043, .F. ) ;
#1857 = CARTESIAN_POINT ( 'NONE',  ( 0.000000000000000000, -84.99999999999998579, 1.499999999999999778 ) ) ;
#1858 = EDGE_CURVE ( 'NONE', #1382, #2217, #1378, .T. ) ;
#1859 = FACE_OUTER_BOUND ( 'NONE', #2664, .T. ) ;
#1860 = ORIENTED_EDGE ( 'NONE', *, *, #2657, .F. ) ;
#1861 = DIRECTION ( 'NONE',  ( 0.000000000000000000, 1.000000000000000000, 0.000000000000000000 ) ) ;
#1862 = DIRECTION ( 'NONE',  ( -1.000000000000000000, 0.000000000000000000, 0.000000000000000000 ) ) ;
#1863 = CARTESIAN_POINT ( 'NONE',  ( 2.500000000000008438, -69.83207023104499456, -4.330127018922187432 ) ) ;
#1864 = APPLICATION_CONTEXT ( 'automotive_design' ) ;
#1865 = VERTEX_POINT ( 'NONE', #3147 ) ;
#1866 = DIRECTION ( 'NONE',  ( -0.000000000000000000, 1.000000000000000000, -0.000000000000000000 ) ) ;
#1867 = PRESENTATION_STYLE_ASSIGNMENT (( #2406 ) ) ;
#1868 = CARTESIAN_POINT ( 'NONE',  ( 0.6766787981060014001, 7.476722154948000743, 4.965272001127371659 ) ) ;
#1869 = CARTESIAN_POINT ( 'NONE',  ( -11.39999999999999680, -50.00000000000000000, -1.366666666666159768 ) ) ;
#1870 = CARTESIAN_POINT ( 'NONE',  ( -4.966432541228214426, -5.620714496023337503, -0.6691698110145376521 ) ) ;
#1871 = EDGE_LOOP ( 'NONE', ( #3062, #1326, #2154, #421, #1662, #3162, #2579, #1346, #1546, #2340, #3024 ) ) ;
#1872 = CARTESIAN_POINT ( 'NONE',  ( -5.000232060827701552, 5.589962382322530843, -0.3381422036129833608 ) ) ;
#1873 = CARTESIAN_POINT ( 'NONE',  ( 11.40000778997679021, -50.00000000000000000, -0.2924664341912772692 ) ) ;
#1874 = EDGE_CURVE ( 'NONE', #439, #1087, #313, .T. ) ;
#1875 = B_SPLINE_CURVE_WITH_KNOTS ( 'NONE', 3,
 ( #1601, #662, #140, #126, #875, #393 ),
 .UNSPECIFIED., .F., .F.,
 ( 4, 2, 4 ),
 ( 0.0004720815379052808731, 0.0007077329675634565264, 0.0009433843972216321254 ),
 .UNSPECIFIED. ) ;
#1876 = DIRECTION ( 'NONE',  ( 0.000000000000000000, 0.000000000000000000, 1.000000000000000000 ) ) ;
#1877 = EDGE_LOOP ( 'NONE', ( #825, #976, #2859, #766, #2910, #2212, #326, #1284, #2054, #853, #1860, #601 ) ) ;
#1878 = FILL_AREA_STYLE_COLOUR ( '', #1905 ) ;
#1879 = ADVANCED_FACE ( 'NONE', ( #1701 ), #2962, .F. ) ;
#1880 = ADVANCED_FACE ( 'NONE', ( #922 ), #1157, .F. ) ;
#1881 = DIRECTION ( 'NONE',  ( 0.000000000000000000, 0.000000000000000000, 1.000000000000000000 ) ) ;
#1882 = CARTESIAN_POINT ( 'NONE',  ( -0.3000000000000161982, -117.6667274285785112, 0.8135312234519368468 ) ) ;
#1883 = VERTEX_POINT ( 'NONE', #1206 ) ;
#1884 = EDGE_CURVE ( 'NONE', #1853, #900, #1453, .T. ) ;
#1885 = CARTESIAN_POINT ( 'NONE',  ( 0.000000000000000000, -72.50000000000001421, -2.500000000000000444 ) ) ;
#1886 = SURFACE_STYLE_FILL_AREA ( #2157 ) ;
#1887 = CARTESIAN_POINT ( 'NONE',  ( -5.742338339643776379, -50.00000000000000000, 9.960716663318299524 ) ) ;
#1888 = CARTESIAN_POINT ( 'NONE',  ( -0.3369232893658926642, -7.494324649304657804, -4.991499248304590353 ) ) ;
#1889 = PRODUCT_RELATED_PRODUCT_CATEGORY ( 'part', '', ( #357 ) ) ;
#1890 = CARTESIAN_POINT ( 'NONE',  ( -0.3000000000000161982, -114.9999999999982236, 0.9539392014169767453 ) ) ;
#1891 = CIRCLE ( 'NONE', #2370, 0.4999999999999813483 ) ;
#1892 = CARTESIAN_POINT ( 'NONE',  ( -11.30825875096001454, -50.00000000000000000, 1.490875164968288757 ) ) ;
#1893 = ORIENTED_EDGE ( 'NONE', *, *, #1517, .T. ) ;
#1894 = CARTESIAN_POINT ( 'NONE',  ( -5.000000000000000000, 24.40983005625052726, 10.00000000000000178 ) ) ;
#1895 = VERTEX_POINT ( 'NONE', #3182 ) ;
#1896 = B_SPLINE_CURVE_WITH_KNOTS ( 'NONE', 3,
 ( #537, #2583, #265, #2339, #1545, #2551, #1075, #1592, #1288, #1040, #2606, #2355, #2304, #2053, #3061, #924, #1142, #1359, #2408, #655, #1870, #896, #2373, #2177, #2424, #148, #2640, #1111, #385, #2879, #2625, #1922, #2128, #418, #668, #1425, #640, #1888, #1641, #351 ),
 .UNSPECIFIED., .F., .F.,
 ( 4, 2, 2, 2, 2, 2, 2, 2, 2, 2, 2, 2, 2, 2, 2, 2, 2, 2, 2, 4 ),
 ( 0.000000000000000000, 0.001009991476537153501, 0.002019982953074307436, 0.003029974429611462239, 0.004039965906148617475, 0.005049957382685771844, 0.006059948859222927947, 0.007069940335760082316, 0.007574936074028659934, 0.008079931812297236685, 0.009089923288834390186, 0.01009991476537154195, 0.01110990624190869892, 0.01211989771844585242, 0.01312988919498300593, 0.01363488493325158528, 0.01413988067152016116, 0.01514987214805731987, 0.01565486788632589749, 0.01615986362459447684 ),
 .UNSPECIFIED. ) ;
#1897 = CARTESIAN_POINT ( 'NONE',  ( -1.464466094067259139, -67.50000000000000000, 2.499999999999997780 ) ) ;
#1898 = EDGE_CURVE ( 'NONE', #1146, #2611, #2608, .T. ) ;
#1899 = CARTESIAN_POINT ( 'NONE',  ( 2.250215587473118450, -50.00000000000000000, 8.376503107919017310 ) ) ;
#1900 = DIRECTION ( 'NONE',  ( 1.000000000000000000, 0.000000000000000000, -0.000000000000000000 ) ) ;
#1901 = ORIENTED_EDGE ( 'NONE', *, *, #909, .F. ) ;
#1902 = VECTOR ( 'NONE', #2033, 1000.000000000000000 ) ;
#1903 = DIRECTION ( 'NONE',  ( -0.000000000000000000, -0.000000000000000000, 1.000000000000000000 ) ) ;
#1904 =( NAMED_UNIT ( * ) PLANE_ANGLE_UNIT ( ) SI_UNIT ( $, .RADIAN. ) );
#1905 = COLOUR_RGB ( '',0.8941176470588234615, 0.8941176470588234615, 0.8941176470588234615 ) ;
#1906 = CARTESIAN_POINT ( 'NONE',  ( -1.492255338562904043, -50.00000000000000000, 11.39999999999999680 ) ) ;
#1907 = FILL_AREA_STYLE ('',( #2927 ) ) ;
#1908 = CIRCLE ( 'NONE', #1962, 2.500000000000000444 ) ;
#1909 = CARTESIAN_POINT ( 'NONE',  ( -2.300000000000000266, -67.40000000000000568, 4.600000000000001421 ) ) ;
#1910 = CARTESIAN_POINT ( 'NONE',  ( 11.40000778997679198, -47.20000000000001705, -0.2924664341912773247 ) ) ;
#1911 = VERTEX_POINT ( 'NONE', #1223 ) ;
#1912 = CARTESIAN_POINT ( 'NONE',  ( -1.997648066307399439, -71.53698439035578360, -4.589990637419044006 ) ) ;
#1913 = ADVANCED_FACE ( 'NONE', ( #3209 ), #1955, .T. ) ;
#1914 = ORIENTED_EDGE ( 'NONE', *, *, #618, .T. ) ;
#1915 = CARTESIAN_POINT ( 'NONE',  ( -0.1655869666764216153, -67.50000000000001421, -5.000000000000000000 ) ) ;
#1916 = CARTESIAN_POINT ( 'NONE',  ( 8.572276570257084671, -50.00000000000000000, 0.7042094815225934390 ) ) ;
#1917 = CARTESIAN_POINT ( 'NONE',  ( 8.600005876649037262, -50.00000000000000000, -0.2541998246239300374 ) ) ;
#1918 = ORIENTED_EDGE ( 'NONE', *, *, #2868, .F. ) ;
#1919 = EDGE_CURVE ( 'NONE', #102, #277, #1529, .T. ) ;
#1920 = CARTESIAN_POINT ( 'NONE',  ( -4.996981400519024952, -48.50997913539912076, 0.1986267936440539450 ) ) ;
#1921 = CARTESIAN_POINT ( 'NONE',  ( -11.37702123033528778, -50.00000000000000000, 0.7471912688805022462 ) ) ;
#1922 = CARTESIAN_POINT ( 'NONE',  ( -2.257837506661119154, -7.153666188643283519, -4.464160652961850495 ) ) ;
#1923 = DIRECTION ( 'NONE',  ( 0.000000000000000000, 0.000000000000000000, -1.000000000000000000 ) ) ;
#1924 = EDGE_CURVE ( 'NONE', #2713, #821, #2239, .T. ) ;
#1925 = CARTESIAN_POINT ( 'NONE',  ( -5.742338339643776379, -50.00000000000000000, 9.960716663318299524 ) ) ;
#1926 = VERTEX_POINT ( 'NONE', #2911 ) ;
#1927 = CARTESIAN_POINT ( 'NONE',  ( 8.489369361306732031, -47.20000000000001705, 1.403517616196621409 ) ) ;
#1928 = EDGE_CURVE ( 'NONE', #2713, #97, #773, .T. ) ;
#1929 = CARTESIAN_POINT ( 'NONE',  ( 0.000000000000000000, 0.000000000000000000, 18.00000000000000355 ) ) ;
#1930 = CARTESIAN_POINT ( 'NONE',  ( 4.965855707945498132, -5.621220898751191797, -0.6727113530297602617 ) ) ;
#1931 = ORIENTED_EDGE ( 'NONE', *, *, #1272, .F. ) ;
#1932 = CARTESIAN_POINT ( 'NONE',  ( 0.3471650268615566470, -64.00752696620394033, 4.990975288187766701 ) ) ;
#1933 = FACE_OUTER_BOUND ( 'NONE', #2427, .T. ) ;
#1934 = CARTESIAN_POINT ( 'NONE',  ( 0.000000000000000000, 30.00000000000000000, 10.00000000000000000 ) ) ;
#1935 = CARTESIAN_POINT ( 'NONE',  ( 2.594030646330690359, -75.41843215906500575, 4.286313293421137871 ) ) ;
#1936 = CARTESIAN_POINT ( 'NONE',  ( -7.500000000000000888, 30.00000000000000000, 18.00000000000000355 ) ) ;
#1937 = CARTESIAN_POINT ( 'NONE',  ( 8.599999999999996092, -47.20000000000001705, -0.5466666666666269991 ) ) ;
#1938 = CARTESIAN_POINT ( 'NONE',  ( 4.784761898981735762, -49.60847529508066600, 1.451366868840367808 ) ) ;
#1939 = VECTOR ( 'NONE', #1203, 1000.000000000000000 ) ;
#1940 = CARTESIAN_POINT ( 'NONE',  ( -11.39999999999999680, -50.00000000000000000, -1.400000000000000133 ) ) ;
#1941 = CARTESIAN_POINT ( 'NONE',  ( 6.877134118866901957, -52.79999999999999716, 5.285102517562147995 ) ) ;
#1942 = VECTOR ( 'NONE', #760, 1000.000000000000000 ) ;
#1943 = EDGE_LOOP ( 'NONE', ( #1856, #471, #579 ) ) ;
#1944 = CARTESIAN_POINT ( 'NONE',  ( -6.877134118866000456, -50.00000000000000000, 5.285102517561346858 ) ) ;
#1945 =( LENGTH_UNIT ( ) NAMED_UNIT ( * ) SI_UNIT ( .MILLI., .METRE. ) );
#1946 = PRESENTATION_LAYER_ASSIGNMENT (  '', '', ( #2688 ) ) ;
#1947 = CARTESIAN_POINT ( 'NONE',  ( 10.61784491273702180, -48.73341048396265052, -0.6178437967800165520 ) ) ;
#1948 = ADVANCED_FACE ( 'NONE', ( #1654 ), #901, .T. ) ;
#1949 = ORIENTED_EDGE ( 'NONE', *, *, #2025, .T. ) ;
#1950 = CARTESIAN_POINT ( 'NONE',  ( 5.000000000000000000, -66.68337520964459486, 0.1770536369485830597 ) ) ;
#1951 = CARTESIAN_POINT ( 'NONE',  ( 5.000000000000000000, 24.40983005625052726, 10.00000000000000178 ) ) ;
#1952 = PRODUCT_RELATED_PRODUCT_CATEGORY ( 'part', '', ( #654 ) ) ;
#1953 = CARTESIAN_POINT ( 'NONE',  ( 7.500000000000000000, 9.184850993605147944E-16, 18.00000000000000355 ) ) ;
#1954 = CARTESIAN_POINT ( 'NONE',  ( 8.572527594031472993E-15, -70.00000000000000000, 10.00000000000000000 ) ) ;
#1955 = CYLINDRICAL_SURFACE ( 'NONE', #945, 7.500000000000000000 ) ;
#1956 = CARTESIAN_POINT ( 'NONE',  ( 7.005833569765147040, -52.79999999999999716, 9.116201041261453142 ) ) ;
#1957 = VECTOR ( 'NONE', #1685, 1000.000000000000000 ) ;
#1958 = DIRECTION ( 'NONE',  ( -0.000000000000000000, -0.000000000000000000, 1.000000000000000000 ) ) ;
#1959 = CARTESIAN_POINT ( 'NONE',  ( -9.199433601068362165, -51.18229052107376020, 0.7695943483570758525 ) ) ;
#1960 = MECHANICAL_DESIGN_GEOMETRIC_PRESENTATION_REPRESENTATION (  '', ( #480 ), #425 ) ;
#1961 = CARTESIAN_POINT ( 'NONE',  ( 5.285102517541700351, -52.79999999999999716, 6.877134118846478295 ) ) ;
#1962 = AXIS2_PLACEMENT_3D ( 'NONE', #2740, #516, #1214 ) ;
#1963 = EDGE_LOOP ( 'NONE', ( #631, #1914, #799, #582 ) ) ;
#1964 = CARTESIAN_POINT ( 'NONE',  ( -8.599999999999996092, -47.20000000000001705, -1.366666666666159546 ) ) ;
#1965 = EDGE_CURVE ( 'NONE', #123, #821, #999, .T. ) ;
#1966 = DIRECTION ( 'NONE',  ( 1.000000000000000000, 0.000000000000000000, 0.000000000000000000 ) ) ;
#1967 = EDGE_CURVE ( 'NONE', #403, #1290, #1570, .T. ) ;
#1968 = DIRECTION ( 'NONE',  ( 0.000000000000000000, 0.000000000000000000, 1.000000000000000000 ) ) ;
#1969 = VERTEX_POINT ( 'NONE', #2153 ) ;
#1970 = CARTESIAN_POINT ( 'NONE',  ( -7.500000000000000000, 0.000000000000000000, 10.00000000000000000 ) ) ;
#1971 = DIRECTION ( 'NONE',  ( -0.000000000000000000, -0.000000000000000000, -1.000000000000000000 ) ) ;
#1972 = DIRECTION ( 'NONE',  ( 0.000000000000000000, 0.000000000000000000, 1.000000000000000000 ) ) ;
#1973 = ORIENTED_EDGE ( 'NONE', *, *, #291, .T. ) ;
#1974 = CARTESIAN_POINT ( 'NONE',  ( -4.772823865982902092, -49.80222060004894757, -1.490154340647099174 ) ) ;
#1975 = CARTESIAN_POINT ( 'NONE',  ( 11.03470001049119453, -50.00000000000000000, 2.958453039085983338 ) ) ;
#1976 = CARTESIAN_POINT ( 'NONE',  ( 2.982843918280273510, -50.00000000000000000, 11.10373667793903252 ) ) ;
#1977 = DIRECTION ( 'NONE',  ( 1.000000000000000000, 0.000000000000000000, 0.000000000000000000 ) ) ;
#1978 = CARTESIAN_POINT ( 'NONE',  ( -5.285102517542626721, -52.79999999999999716, 6.877134118847253674 ) ) ;
#1979 = VERTEX_POINT ( 'NONE', #2680 ) ;
#1980 = CARTESIAN_POINT ( 'NONE',  ( 8.530791689320604831, -50.00000000000000000, 1.124695299888175182 ) ) ;
#1981 = CARTESIAN_POINT ( 'NONE',  ( -6.610444160707455418E-15, -72.50000000000009948, -5.000000000000047962 ) ) ;
#1982 = FACE_OUTER_BOUND ( 'NONE', #135, .T. ) ;
#1983 = EDGE_CURVE ( 'NONE', #1333, #1349, #1096, .T. ) ;
#1984 = CARTESIAN_POINT ( 'NONE',  ( 0.000000000000000000, 30.00000000000000000, 10.00000000000000000 ) ) ;
#1985 = CARTESIAN_POINT ( 'NONE',  ( -11.36325033731739076, -47.20000000000001705, 0.9334869871344717573 ) ) ;
#1986 = DIRECTION ( 'NONE',  ( 0.000000000000000000, 0.000000000000000000, 1.000000000000000000 ) ) ;
#1987 = CARTESIAN_POINT ( 'NONE',  ( 4.325820249441205689, -74.16453108894374679, 2.526170042365373014 ) ) ;
#1988 = ADVANCED_FACE ( 'NONE', ( #3129, #96 ), #2419, .F. ) ;
#1989 = CARTESIAN_POINT ( 'NONE',  ( -8.600005876649037262, -50.00000000000000000, -0.2541998246238979520 ) ) ;
#1990 = CARTESIAN_POINT ( 'NONE',  ( 11.40000778997679021, -50.00000000000000000, -0.2924664341912772692 ) ) ;
#1991 = LINE ( 'NONE', #1703, #193 ) ;
#1992 = CARTESIAN_POINT ( 'NONE',  ( -8.609154349732479616, -50.54332563323215055, 1.294262817215226846 ) ) ;
#1993 = CARTESIAN_POINT ( 'NONE',  ( 11.39999532361432522, -52.79999999999999716, 0.1755699507458462760 ) ) ;
#1994 = ORIENTED_EDGE ( 'NONE', *, *, #104, .F. ) ;
#1995 = CARTESIAN_POINT ( 'NONE',  ( 5.285102517541700351, -47.20000000000001705, 6.877134118846478295 ) ) ;
#1996 = AXIS2_PLACEMENT_3D ( 'NONE', #206, #3242, #175 ) ;
#1997 = DIRECTION ( 'NONE',  ( 0.000000000000000000, -1.000000000000000000, 0.000000000000000000 ) ) ;
#1998 = AXIS2_PLACEMENT_3D ( 'NONE', #2484, #3208, #2758 ) ;
#1999 = DIRECTION ( 'NONE',  ( -0.000000000000000000, -1.000000000000000000, -0.000000000000000000 ) ) ;
#2000 = CIRCLE ( 'NONE', #304, 2.500000000000000000 ) ;
#2001 = CARTESIAN_POINT ( 'NONE',  ( 8.572276570257082895, -47.20000000000001705, 0.7042094815225934390 ) ) ;
#2002 = CARTESIAN_POINT ( 'NONE',  ( -11.03726195774814478, -49.04331167652343026, -1.037261957748144114 ) ) ;
#2003 = DIRECTION ( 'NONE',  ( 1.000000000000000000, -0.000000000000000000, -0.000000000000000000 ) ) ;
#2004 = EDGE_CURVE ( 'NONE', #2753, #810, #669, .T. ) ;
#2005 = DIRECTION ( 'NONE',  ( -0.000000000000000000, 0.000000000000000000, 1.000000000000000000 ) ) ;
#2006 = CARTESIAN_POINT ( 'NONE',  ( 9.959683570761143301, -52.79999999999999716, 5.743837162466679302 ) ) ;
#2007 = CARTESIAN_POINT ( 'NONE',  ( -1.492255338562904043, -50.00000000000000000, 11.39999999999999680 ) ) ;
#2008 = DIRECTION ( 'NONE',  ( -1.000000000000000000, 0.000000000000000000, 0.000000000000000000 ) ) ;
#2009 = ADVANCED_FACE ( 'NONE', ( #1635, #2366 ), #2874, .F. ) ;
#2010 = CIRCLE ( 'NONE', #2431, 2.300000000000000266 ) ;
#2011 = CARTESIAN_POINT ( 'NONE',  ( -8.599999999999996092, -52.79999999999999716, -0.5466666666666361030 ) ) ;
#2012 = B_SPLINE_CURVE_WITH_KNOTS ( 'NONE', 3,
 ( #2980, #1178, #2929, #2209, #419, #1161 ),
 .UNSPECIFIED., .F., .F.,
 ( 4, 2, 4 ),
 ( 1.973474095026720747E-07, 0.0002361394426573918174, 0.0004720815379052809273 ),
 .UNSPECIFIED. ) ;
#2013 = ORIENTED_EDGE ( 'NONE', *, *, #3087, .T. ) ;
#2014 = AXIS2_PLACEMENT_3D ( 'NONE', #475, #2987, #2235 ) ;
#2015 = DIRECTION ( 'NONE',  ( -0.000000000000000000, -0.000000000000000000, -1.000000000000000000 ) ) ;
#2016 = PRODUCT_CONTEXT ( 'NONE', #2986, 'mechanical' ) ;
#2017 = MECHANICAL_DESIGN_GEOMETRIC_PRESENTATION_REPRESENTATION (  '', ( #2798 ), #1586 ) ;
#2018 = CARTESIAN_POINT ( 'NONE',  ( 2.541265623391468331, -7.062137256042765543, 4.317949725309306430 ) ) ;
#2019 = CARTESIAN_POINT ( 'NONE',  ( -4.856148773929144902, -50.91572476600896380, 1.192039989181127080 ) ) ;
#2020 = DIRECTION ( 'NONE',  ( 0.000000000000000000, 1.000000000000000000, 0.000000000000000000 ) ) ;
#2021 = LINE ( 'NONE', #2064, #1942 ) ;
#2022 = CARTESIAN_POINT ( 'NONE',  ( 0.2999999999999837796, -116.3333805752222929, -0.8840510694876462239 ) ) ;
#2023 = CARTESIAN_POINT ( 'NONE',  ( 11.39999999999999680, -52.79999999999999716, -1.093333333333372126 ) ) ;
#2024 = ORIENTED_EDGE ( 'NONE', *, *, #98, .F. ) ;
#2025 = EDGE_CURVE ( 'NONE', #1036, #903, #1620, .T. ) ;
#2026 = CARTESIAN_POINT ( 'NONE',  ( 5.285102517541700351, -50.00000000000000000, 6.877134118846478295 ) ) ;
#2027 = ORIENTED_EDGE ( 'NONE', *, *, #692, .T. ) ;
#2028 = CARTESIAN_POINT ( 'NONE',  ( 4.815309899926791815, -50.66728354398328094, -1.346969744587360074 ) ) ;
#2029 = DIRECTION ( 'NONE',  ( 0.000000000000000000, 1.000000000000000000, 0.000000000000000000 ) ) ;
#2030 = EDGE_CURVE ( 'NONE', #1911, #1630, #395, .T. ) ;
#2031 = CARTESIAN_POINT ( 'NONE',  ( -4.977308113077120844, -51.42299734723061277, 0.4845947803478808380 ) ) ;
#2032 = UNCERTAINTY_MEASURE_WITH_UNIT (LENGTH_MEASURE( 1.000000000000000082E-05 ), #382, 'distance_accuracy_value', 'NONE');
#2033 = DIRECTION ( 'NONE',  ( -0.000000000000000000, -0.000000000000000000, -1.000000000000000000 ) ) ;
#2034 = DIRECTION ( 'NONE',  ( 1.000000000000000000, 0.000000000000000000, -0.000000000000000000 ) ) ;
#2035 = CARTESIAN_POINT ( 'NONE',  ( 2.499999999999999556, 0.000000000000000000, 10.00000000000000000 ) ) ;
#2036 = CARTESIAN_POINT ( 'NONE',  ( -8.599999999999996092, -50.00000000000000000, -1.639999999999997460 ) ) ;
#2037 = ORIENTED_EDGE ( 'NONE', *, *, #929, .F. ) ;
#2038 = SURFACE_STYLE_FILL_AREA ( #780 ) ;
#2039 = CARTESIAN_POINT ( 'NONE',  ( -2.347667281524951198E-13, -114.6999999999962228, 1.015000000000727765 ) ) ;
#2040 =( REPRESENTATION_RELATIONSHIP ('NONE','NONE', #545, #2799 ) REPRESENTATION_RELATIONSHIP_WITH_TRANSFORMATION ( #523 )SHAPE_REPRESENTATION_RELATIONSHIP( ) );
#2041 = CARTESIAN_POINT ( 'NONE',  ( 0.000000000000000000, -125.0000000000000000, 0.000000000000000000 ) ) ;
#2042 = ORIENTED_EDGE ( 'NONE', *, *, #2132, .F. ) ;
#2043 = CARTESIAN_POINT ( 'NONE',  ( 4.856137924134493744, -50.91569030856719280, -1.192091538463844191 ) ) ;
#2044 = CARTESIAN_POINT ( 'NONE',  ( -0.6937423435388923032, -75.96229638456773614, 4.954702760404292583 ) ) ;
#2045 = CARTESIAN_POINT ( 'NONE',  ( -5.000000000000000000, 30.00000000000000000, 18.00000000000000355 ) ) ;
#2046 = DIRECTION ( 'NONE',  ( -0.000000000000000000, -1.000000000000000000, 0.000000000000000000 ) ) ;
#2047 = CIRCLE ( 'NONE', #1098, 2.499999999999999556 ) ;
#2048 = CARTESIAN_POINT ( 'NONE',  ( 8.485280282859413603, -50.00000000000000000, 1.400000000000001021 ) ) ;
#2049 = CARTESIAN_POINT ( 'NONE',  ( 8.599999999999996092, -52.79999999999999716, -1.639999999999997460 ) ) ;
#2050 = ORIENTED_EDGE ( 'NONE', *, *, #2030, .T. ) ;
#2051 = DIRECTION ( 'NONE',  ( 0.000000000000000000, 0.000000000000000000, 1.000000000000000000 ) ) ;
#2052 = CARTESIAN_POINT ( 'NONE',  ( 8.600005876649037262, -50.00000000000000000, -0.2541998246239300374 ) ) ;
#2053 = CARTESIAN_POINT ( 'NONE',  ( -4.728889495302424528, -5.823500886956166411, 1.655898480698586139 ) ) ;
#2054 = ORIENTED_EDGE ( 'NONE', *, *, #273, .F. ) ;
#2055 = DIRECTION ( 'NONE',  ( -0.000000000000000000, -0.000000000000000000, -1.000000000000000000 ) ) ;
#2056 = CARTESIAN_POINT ( 'NONE',  ( -11.03470001049236160, -47.20000000000001705, 2.958453039083849045 ) ) ;
#2057 = AXIS2_PLACEMENT_3D ( 'NONE', #3145, #2650, #2120 ) ;
#2058 = ORIENTED_EDGE ( 'NONE', *, *, #1965, .F. ) ;
#2059 = EDGE_CURVE ( 'NONE', #2708, #2182, #1740, .T. ) ;
#2060 = CARTESIAN_POINT ( 'NONE',  ( -4.475554532957456644, -74.00082003167284483, 2.251442214368888362 ) ) ;
#2062 = EDGE_CURVE ( 'NONE', #1810, #2412, #2269, .T. ) ;
#2061 = UNCERTAINTY_MEASURE_WITH_UNIT (LENGTH_MEASURE( 1.000000000000000082E-05 ), #80, 'distance_accuracy_value', 'NONE');
#2063 = VECTOR ( 'NONE', #339, 1000.000000000000000 ) ;
#2064 = CARTESIAN_POINT ( 'NONE',  ( 0.000000000000000000, -84.99999999999998579, 2.300000000000000266 ) ) ;
#2065 = AXIS2_PLACEMENT_3D ( 'NONE', #1383, #1631, #374 ) ;
#2066 = APPLICATION_PROTOCOL_DEFINITION ( 'draft international standard', 'automotive_design', 1998, #279 ) ;
#2067 = CARTESIAN_POINT ( 'NONE',  ( 6.123233995736765296E-16, -80.00000000000000000, -4.999999999999999112 ) ) ;
#2068 = CARTESIAN_POINT ( 'NONE',  ( -8.599999999999996092, -50.00000000000000000, -1.093333333333363022 ) ) ;
#2069 = ORIENTED_EDGE ( 'NONE', *, *, #1789, .F. ) ;
#2070 = CARTESIAN_POINT ( 'NONE',  ( 4.999999999999999112, -73.31662479035541935, 0.000000000000000000 ) ) ;
#2071 =( LENGTH_UNIT ( ) NAMED_UNIT ( * ) SI_UNIT ( .MILLI., .METRE. ) );
#2072 = CARTESIAN_POINT ( 'NONE',  ( -0.07897820435409848294, -119.2999999999982350, 0.7850000000000507683 ) ) ;
#2073 = CARTESIAN_POINT ( 'NONE',  ( 1.464466094067265800, -72.50000000000001421, -2.499999999999999556 ) ) ;
#2074 = ORIENTED_EDGE ( 'NONE', *, *, #942, .T. ) ;
#2075 = CARTESIAN_POINT ( 'NONE',  ( 6.124525076959063726E-16, 7.500000000000000000, -4.999999999999999112 ) ) ;
#2076 = ITEM_DEFINED_TRANSFORMATION ( 'NONE', 'NONE', #266,  #1692 ) ;
#2077 = CARTESIAN_POINT ( 'NONE',  ( -11.37702123033536061, -47.20000000000001705, 0.7471912688805021352 ) ) ;
#2078 = ORIENTED_EDGE ( 'NONE', *, *, #3043, .F. ) ;
#2079 = B_SPLINE_CURVE_WITH_KNOTS ( 'NONE', 3,
 ( #324, #1774, #1513, #1824, #270, #2262, #2831, #3083, #287, #1279, #577, #1580, #3018, #2327, #1808, #2814, #2031, #2524, #3047, #1261, #2019, #24, #3030, #525, #1066, #2592, #3272, #1550 ),
 .UNSPECIFIED., .F., .F.,
 ( 4, 2, 2, 2, 2, 2, 2, 2, 2, 2, 2, 2, 2, 4 ),
 ( 0.000000000000000000, 0.0002948077093299257545, 0.0005896154186598515090, 0.0008844231279897772635, 0.001179230837319703018, 0.001768846255979540866, 0.002358461674639378714, 0.002653269383969297963, 0.002948077093299216345, 0.003537692511959054844, 0.003832500221288973660, 0.004127307930618892041, 0.004422115639948811724, 0.004716923349278730540 ),
 .UNSPECIFIED. ) ;
#2080 = CARTESIAN_POINT ( 'NONE',  ( -2.309991845038993574, -75.54707137493313951, 4.447043502685488647 ) ) ;
#2081 = EDGE_CURVE ( 'NONE', #2538, #1754, #2846, .T. ) ;
#2082 = FACE_OUTER_BOUND ( 'NONE', #1398, .T. ) ;
#2083 = VERTEX_POINT ( 'NONE', #2202 ) ;
#2084 = CARTESIAN_POINT ( 'NONE',  ( 0.000000000000000000, 0.000000000000000000, 18.00000000000000355 ) ) ;
#2085 = CARTESIAN_POINT ( 'NONE',  ( 4.331939449206418935, -50.00000000000000000, 7.514224851275112194 ) ) ;
#2086 = ORIENTED_EDGE ( 'NONE', *, *, #1272, .T. ) ;
#2087 = EDGE_CURVE ( 'NONE', #1541, #1748, #1364, .T. ) ;
#2088 = DIRECTION ( 'NONE',  ( 0.000000000000000000, 0.000000000000000000, 1.000000000000000000 ) ) ;
#2089 = DIRECTION ( 'NONE',  ( 0.000000000000000000, 0.000000000000000000, 1.000000000000000000 ) ) ;
#2090 = CARTESIAN_POINT ( 'NONE',  ( 0.000000000000000000, -125.0000000000000000, 0.000000000000000000 ) ) ;
#2091 = DIRECTION ( 'NONE',  ( -0.000000000000000000, -0.000000000000000000, -1.000000000000000000 ) ) ;
#2092 = ORIENTED_EDGE ( 'NONE', *, *, #1758, .F. ) ;
#2093 = FACE_OUTER_BOUND ( 'NONE', #2388, .T. ) ;
#2094 = CARTESIAN_POINT ( 'NONE',  ( 5.285102517541700351, -47.20000000000001705, 6.877134118846478295 ) ) ;
#2095 = DIRECTION ( 'NONE',  ( 0.000000000000000000, 0.000000000000000000, -1.000000000000000000 ) ) ;
#2096 = AXIS2_PLACEMENT_3D ( 'NONE', #2857, #599, #95 ) ;
#2097 = CARTESIAN_POINT ( 'NONE',  ( -8.160064090060583197, -50.00000000000000000, 2.773119917861301964 ) ) ;
#2098 = ORIENTED_EDGE ( 'NONE', *, *, #320, .F. ) ;
#2099 = CARTESIAN_POINT ( 'NONE',  ( 2.500000000000004441, -70.00000000000000000, 0.000000000000000000 ) ) ;
#2100 = CARTESIAN_POINT ( 'NONE',  ( -8.489369361306263073, -50.00000000000000000, 1.403517616197273554 ) ) ;
#2101 = VERTEX_POINT ( 'NONE', #2463 ) ;
#2102 = AXIS2_PLACEMENT_3D ( 'NONE', #1954, #479, #2203 ) ;
#2103 = DIRECTION ( 'NONE',  ( 0.000000000000000000, 0.000000000000000000, 1.000000000000000000 ) ) ;
#2104 = DIRECTION ( 'NONE',  ( 1.000000000000000000, 0.000000000000000000, 0.000000000000000000 ) ) ;
#2105 = AXIS2_PLACEMENT_3D ( 'NONE', #614, #1862, #2818 ) ;
#2106 = CARTESIAN_POINT ( 'NONE',  ( 4.480628327518417109, 6.016609984030584890, -2.242680489316260850 ) ) ;
#2107 = CARTESIAN_POINT ( 'NONE',  ( -0.1739454948912136090, -64.00000000000001421, 5.000000000000000000 ) ) ;
#2108 = DIRECTION ( 'NONE',  ( 0.000000000000000000, 0.000000000000000000, 1.000000000000000000 ) ) ;
#2109 = VERTEX_POINT ( 'NONE', #2499 ) ;
#2110 = CARTESIAN_POINT ( 'NONE',  ( -0.8431454290909620175, 7.454306392314355989, -4.931260737871609123 ) ) ;
#2111 = EDGE_CURVE ( 'NONE', #900, #1046, #699, .T. ) ;
#2112 = CARTESIAN_POINT ( 'NONE',  ( 11.39999532361432522, -47.20000000000001705, 0.1755699507458462760 ) ) ;
#2113 = CARTESIAN_POINT ( 'NONE',  ( -4.990448535730164004, -73.33113742485521414, 0.3539254956240150962 ) ) ;
#2114 = AXIS2_PLACEMENT_3D ( 'NONE', #2990, #222, #1220 ) ;
#2115 = DIRECTION ( 'NONE',  ( 0.000000000000000000, 0.000000000000000000, 1.000000000000000000 ) ) ;
#2116 = ORIENTED_EDGE ( 'NONE', *, *, #986, .F. ) ;
#2117 = VECTOR ( 'NONE', #1485, 1000.000000000000000 ) ;
#2118 = CARTESIAN_POINT ( 'NONE',  ( -2.499999999999992006, -69.83441493831065827, -4.330127018922196314 ) ) ;
#2119 = DIRECTION ( 'NONE',  ( -0.000000000000000000, -0.000000000000000000, 1.000000000000000000 ) ) ;
#2120 = DIRECTION ( 'NONE',  ( 1.000000000000000000, 0.000000000000000000, 0.000000000000000000 ) ) ;
#2121 = COLOUR_RGB ( '',0.8941176470588234615, 0.8941176470588234615, 0.8941176470588234615 ) ;
#2122 = EDGE_LOOP ( 'NONE', ( #1421, #1079, #2069, #1710 ) ) ;
#2123 = CARTESIAN_POINT ( 'NONE',  ( -2.499999999999995559, -71.46446609406727646, -1.464466094067262025 ) ) ;
#2124 = AXIS2_PLACEMENT_3D ( 'NONE', #1356, #2390, #290 ) ;
#2125 = EDGE_CURVE ( 'NONE', #3214, #2870, #3007, .T. ) ;
#2126 = CARTESIAN_POINT ( 'NONE',  ( 4.733269301232542858, 5.819947390767942430, -1.643717648664120068 ) ) ;
#2127 = CARTESIAN_POINT ( 'NONE',  ( -5.000000000000000888, -66.68337520964462328, 0.3546751931833541649 ) ) ;
#2128 = CARTESIAN_POINT ( 'NONE',  ( -2.108823893667861604, -7.199131270151879924, -4.536514892156152889 ) ) ;
#2129 = ORIENTED_EDGE ( 'NONE', *, *, #3177, .T. ) ;
#2130 = CARTESIAN_POINT ( 'NONE',  ( -2.499999999999999556, 0.000000000000000000, 10.00000000000000000 ) ) ;
#2131 = CARTESIAN_POINT ( 'NONE',  ( 7.005833569765714586, -50.00000000000000000, 9.116201041261451365 ) ) ;
#2132 = EDGE_CURVE ( 'NONE', #651, #1093, #1372, .T. ) ;
#2133 = ORIENTED_EDGE ( 'NONE', *, *, #3253, .T. ) ;
#2134 = PRODUCT_DEFINITION_SHAPE ( 'NONE', 'NONE',  #1648 ) ;
#2135 = CARTESIAN_POINT ( 'NONE',  ( -1.658049672226218574, -71.87792464909678358, -4.718635845934137762 ) ) ;
#2136 = EDGE_LOOP ( 'NONE', ( #300, #58 ) ) ;
#2137 = LINE ( 'NONE', #1385, #2227 ) ;
#2138 = CARTESIAN_POINT ( 'NONE',  ( 8.572527594031472993E-15, -70.00000000000000000, 10.00000000000000000 ) ) ;
#2139 = CARTESIAN_POINT ( 'NONE',  ( 8.599999999999996092, -50.00000000000000000, -1.366666666666861873 ) ) ;
#2140 = ORIENTED_EDGE ( 'NONE', *, *, #464, .T. ) ;
#2141 = CARTESIAN_POINT ( 'NONE',  ( -1.464466094067257806, -72.50000000000001421, -2.499999999999999556 ) ) ;
#2142 = CARTESIAN_POINT ( 'NONE',  ( -11.39539595717866405, -50.00000000000000000, 0.3739757293043588504 ) ) ;
#2143 = CARTESIAN_POINT ( 'NONE',  ( -11.39999999999999680, -50.00000000000000000, -0.5466666666666361030 ) ) ;
#2144 = CARTESIAN_POINT ( 'NONE',  ( -0.6741883319902871596, 7.471549563736964217, -4.957238835368188212 ) ) ;
#2145 = CARTESIAN_POINT ( 'NONE',  ( 1.492255338562904043, -50.00000000000000000, 11.39999999999999680 ) ) ;
#2146 = ORIENTED_EDGE ( 'NONE', *, *, #1759, .T. ) ;
#2147 = EDGE_CURVE ( 'NONE', #216, #1541, #2250, .T. ) ;
#2148 = CARTESIAN_POINT ( 'NONE',  ( -2.500000000000000000, 0.000000000000000000, -10.00000000000000000 ) ) ;
#2149 = ADVANCED_FACE ( 'NONE', ( #2975, #743, #3273 ), #3256, .F. ) ;
#2150 = ORIENTED_EDGE ( 'NONE', *, *, #2822, .F. ) ;
#2151 = CARTESIAN_POINT ( 'NONE',  ( -2.499999999999994671, -68.53553390593273775, 1.464466094067261137 ) ) ;
#2152 = DIRECTION ( 'NONE',  ( 0.000000000000000000, 0.000000000000000000, -1.000000000000000000 ) ) ;
#2153 = CARTESIAN_POINT ( 'NONE',  ( 5.000000000000000000, 24.40983005625052726, 18.00000000000000355 ) ) ;
#2154 = ORIENTED_EDGE ( 'NONE', *, *, #1758, .T. ) ;
#2155 = VECTOR ( 'NONE', #412, 1000.000000000000000 ) ;
#2156 = CARTESIAN_POINT ( 'NONE',  ( -0.3000000000000161982, -114.9999999999982236, -2.300000000000000266 ) ) ;
#2157 = FILL_AREA_STYLE ('',( #620 ) ) ;
#2158 = CARTESIAN_POINT ( 'NONE',  ( -2.982843918280285944, -50.00000000000000000, 11.10373667793902541 ) ) ;
#2159 = PRODUCT ( 'Needle Bar', 'Needle Bar', '', ( #2016 ) ) ;
#2160 = CARTESIAN_POINT ( 'NONE',  ( -4.324630367402185982, 6.131366064188266130, 2.529815037953009327 ) ) ;
#2161 = AXIS2_PLACEMENT_3D ( 'NONE', #798, #3040, #1835 ) ;
#2162 = CARTESIAN_POINT ( 'NONE',  ( -9.116201041287103735, -52.79999999999999716, 7.005833569791151128 ) ) ;
#2163 = ORIENTED_EDGE ( 'NONE', *, *, #1533, .T. ) ;
#2164 = CARTESIAN_POINT ( 'NONE',  ( -9.198767304811452661, -48.81800434884508633, 0.7702149575309138463 ) ) ;
#2165 = ADVANCED_FACE ( 'NONE', ( #3207 ), #2450, .T. ) ;
#2166 = VERTEX_POINT ( 'NONE', #714 ) ;
#2167 = CARTESIAN_POINT ( 'NONE',  ( -1.653533745081442907, -68.11807823234784109, -4.720230888861525642 ) ) ;
#2168 = AXIS2_PLACEMENT_3D ( 'NONE', #1249, #2020, #1972 ) ;
#2169 = CARTESIAN_POINT ( 'NONE',  ( -8.530791689320901483, -50.00000000000000000, 1.124695299888049504 ) ) ;
#2170 = DIRECTION ( 'NONE',  ( -0.000000000000000000, -1.000000000000000000, -0.000000000000000000 ) ) ;
#2171 = VERTEX_POINT ( 'NONE', #2729 ) ;
#2172 = VECTOR ( 'NONE', #1119, 1000.000000000000000 ) ;
#2173 = EDGE_CURVE ( 'NONE', #403, #661, #1714, .T. ) ;
#2174 = CARTESIAN_POINT ( 'NONE',  ( 5.000000000000000000, 5.590169943749474513, 18.00000000000000355 ) ) ;
#2175 = AXIS2_PLACEMENT_3D ( 'NONE', #505, #819, #2543 ) ;
#2176 = CARTESIAN_POINT ( 'NONE',  ( 11.40000778997679198, -47.20000000000001705, -0.2924664341912773247 ) ) ;
#2177 = CARTESIAN_POINT ( 'NONE',  ( -4.480628327518417109, -6.016609984030584890, -2.242680489316260850 ) ) ;
#2178 = EDGE_CURVE ( 'NONE', #1969, #1883, #1790, .T. ) ;
#2179 = COLOUR_RGB ( '',0.8941176470588234615, 0.8941176470588234615, 0.8941176470588234615 ) ;
#2180 = CYLINDRICAL_SURFACE ( 'NONE', #1144, 0.2999999999999999889 ) ;
#2181 = CARTESIAN_POINT ( 'NONE',  ( 10.81682914263883610, -50.00000000000000000, 3.675996170187548540 ) ) ;
#2182 = VERTEX_POINT ( 'NONE', #1469 ) ;
#2183 = CARTESIAN_POINT ( 'NONE',  ( 0.1666858246784454212, -72.50000000000002842, -5.000000000000003553 ) ) ;
#2184 = CARTESIAN_POINT ( 'NONE',  ( 4.725421832813011314, -5.824466512821798503, -1.642406358834817004 ) ) ;
#2185 = EDGE_LOOP ( 'NONE', ( #2776, #2570, #267, #1104, #78, #1027, #944, #2331 ) ) ;
#2186 = CARTESIAN_POINT ( 'NONE',  ( 8.572527594031472993E-15, -70.00000000000000000, 10.00000000000000000 ) ) ;
#2187 = CARTESIAN_POINT ( 'NONE',  ( -8.599999999999996092, -50.00000000000000000, -0.5466666666666361030 ) ) ;
#2188 = CARTESIAN_POINT ( 'NONE',  ( 0.1654076819047616553, -67.50000000000000000, -4.999999999999998224 ) ) ;
#2189 = CARTESIAN_POINT ( 'NONE',  ( 10.62090117298859226, -51.26516722440714346, -0.6209000891238516395 ) ) ;
#2190 = CARTESIAN_POINT ( 'NONE',  ( -4.945771905224659371, -48.69008891295303698, -0.7565992915569080823 ) ) ;
#2191 = CARTESIAN_POINT ( 'NONE',  ( 11.25335008359258282, -47.20000000000001705, 1.860476840074028360 ) ) ;
#2192 = SURFACE_SIDE_STYLE ('',( #1160 ) ) ;
#2193 = CARTESIAN_POINT ( 'NONE',  ( -10.76674801461903286, -51.18483196047731809, -0.7667480146190315260 ) ) ;
#2194 = CARTESIAN_POINT ( 'NONE',  ( -5.742338339643776379, -52.79999999999999716, 9.960716663318299524 ) ) ;
#2195 = VERTEX_POINT ( 'NONE', #2237 ) ;
#2196 = CARTESIAN_POINT ( 'NONE',  ( 8.599999999999996092, -50.00000000000000000, -1.366666666666861873 ) ) ;
#2197 = CYLINDRICAL_SURFACE ( 'NONE', #2752, 7.500000000000000000 ) ;
#2198 = CARTESIAN_POINT ( 'NONE',  ( 4.999999999999998224, 30.00000000000000000, 10.00000000000000000 ) ) ;
#2199 = VERTEX_POINT ( 'NONE', #447 ) ;
#2200 = CARTESIAN_POINT ( 'NONE',  ( 4.990448535730164004, -66.66886257514475744, 0.3539254956240222016 ) ) ;
#2201 = FACE_OUTER_BOUND ( 'NONE', #1293, .T. ) ;
#2202 = CARTESIAN_POINT ( 'NONE',  ( -2.499999999999991118, -70.00000000000000000, -4.330127018922196314 ) ) ;
#2203 = DIRECTION ( 'NONE',  ( 1.000000000000000000, 0.000000000000000000, -0.000000000000000000 ) ) ;
#2204 = CARTESIAN_POINT ( 'NONE',  ( -4.999998311775604165, -48.50000562741465870, 0.09894250604207632804 ) ) ;
#2205 = CARTESIAN_POINT ( 'NONE',  ( 5.742338339644331491, -52.79999999999999716, 9.960716663318304853 ) ) ;
#2206 = CARTESIAN_POINT ( 'NONE',  ( 4.945777185212984151, -48.69007577354707905, -0.7564652374250301348 ) ) ;
#2207 = AXIS2_PLACEMENT_3D ( 'NONE', #2921, #394, #3191 ) ;
#2208 = EDGE_CURVE ( 'NONE', #3130, #1156, #3119, .T. ) ;
#2209 = CARTESIAN_POINT ( 'NONE',  ( 0.1568842751130637980, -119.2672622186050262, -0.7728910312014006800 ) ) ;
#2210 = CARTESIAN_POINT ( 'NONE',  ( 11.30825875096042310, -52.79999999999999716, 1.490875164968454625 ) ) ;
#2211 =( REPRESENTATION_RELATIONSHIP ('NONE','NONE', #545, #1236 ) REPRESENTATION_RELATIONSHIP_WITH_TRANSFORMATION ( #3044 )SHAPE_REPRESENTATION_RELATIONSHIP( ) );
#2212 = ORIENTED_EDGE ( 'NONE', *, *, #2272, .T. ) ;
#2213 = EDGE_CURVE ( 'NONE', #2171, #1156, #970, .T. ) ;
#2214 = CARTESIAN_POINT ( 'NONE',  ( 8.582665138674004268, -50.00000000000000000, 0.5636706063485154017 ) ) ;
#2215 = DIRECTION ( 'NONE',  ( 1.000000000000000000, 0.000000000000000000, 0.000000000000000000 ) ) ;
#2216 = CARTESIAN_POINT ( 'NONE',  ( 10.76729745289141604, -48.81576204415910780, -0.7672974528913893977 ) ) ;
#2217 = VERTEX_POINT ( 'NONE', #2744 ) ;
#2218 = CARTESIAN_POINT ( 'NONE',  ( 1.373679055183318676, -64.14932959975399740, 4.819953665648758268 ) ) ;
#2219 = CARTESIAN_POINT ( 'NONE',  ( -8.599996472200352571, -50.00000000000000000, 0.1525981975067654262 ) ) ;
#2220 = CARTESIAN_POINT ( 'NONE',  ( 0.000000000000000000, -67.50000000000000000, -2.500000000000000444 ) ) ;
#2221 = LINE ( 'NONE', #334, #2678 ) ;
#2222 = CARTESIAN_POINT ( 'NONE',  ( -4.856137924134493744, -49.08430969143282141, -1.192091538463844191 ) ) ;
#2223 = CARTESIAN_POINT ( 'NONE',  ( -11.39999999999999680, -52.79999999999999716, -0.5466666666666361030 ) ) ;
#2224 = CARTESIAN_POINT ( 'NONE',  ( 4.793520869840776299, -49.51425668076524289, -1.422568331971221456 ) ) ;
#2225 = CARTESIAN_POINT ( 'NONE',  ( 0.000000000000000000, -80.00000000000000000, 0.000000000000000000 ) ) ;
#2226 = VECTOR ( 'NONE', #1847, 1000.000000000000000 ) ;
#2227 = VECTOR ( 'NONE', #2401, 1000.000000000000000 ) ;
#2228 = CARTESIAN_POINT ( 'NONE',  ( 8.599996472200352571, -52.79999999999999716, 0.1525981975067867147 ) ) ;
#2229 = ORIENTED_EDGE ( 'NONE', *, *, #1924, .T. ) ;
#2230 = CARTESIAN_POINT ( 'NONE',  ( 5.285102517541700351, -50.00000000000000000, 6.877134118846478295 ) ) ;
#2231 = CARTESIAN_POINT ( 'NONE',  ( 2.483169110057957596, -70.33326608521694823, -4.339962428766264146 ) ) ;
#2232 = CARTESIAN_POINT ( 'NONE',  ( 3.772047191027663615, -6.487346954507292374, -3.297239103104800506 ) ) ;
#2233 = EDGE_CURVE ( 'NONE', #890, #365, #174, .T. ) ;
#2234 = EDGE_CURVE ( 'NONE', #1320, #3214, #508, .T. ) ;
#2235 = DIRECTION ( 'NONE',  ( 1.000000000000000000, 0.000000000000000000, 0.000000000000000000 ) ) ;
#2236 = CARTESIAN_POINT ( 'NONE',  ( 8.324422814932070480, -50.00000000000000000, 2.231815450537910639 ) ) ;
#2237 = CARTESIAN_POINT ( 'NONE',  ( 4.999999999999999112, 30.00000000000000000, 18.00000000000000355 ) ) ;
#2238 = CARTESIAN_POINT ( 'NONE',  ( 4.724063086364460595, -73.70412200079239540, 1.668329630282858078 ) ) ;
#2239 = LINE ( 'NONE', #3245, #2902 ) ;
#2240 = CARTESIAN_POINT ( 'NONE',  ( -5.742338339643776379, -52.79999999999999716, 9.960716663318299524 ) ) ;
#2241 = CARTESIAN_POINT ( 'NONE',  ( 0.000000000000000000, -84.99999999999998579, 0.000000000000000000 ) ) ;
#2242 = CARTESIAN_POINT ( 'NONE',  ( -10.00000000000001776, -51.39999999999999858, 1.734719586992576771E-19 ) ) ;
#2243 = CARTESIAN_POINT ( 'NONE',  ( 1.125736483477000061, -52.79999999999999716, 8.599999999999996092 ) ) ;
#2244 = ORIENTED_EDGE ( 'NONE', *, *, #3154, .F. ) ;
#2245 = CARTESIAN_POINT ( 'NONE',  ( -8.489369361306263073, -47.20000000000001705, 1.403517616197273554 ) ) ;
#2246 = CARTESIAN_POINT ( 'NONE',  ( 4.669423702320314895, -5.869651582198522455, -1.795146503317839759 ) ) ;
#2247 = ADVANCED_FACE ( 'NONE', ( #271 ), #2282, .T. ) ;
#2248 = CARTESIAN_POINT ( 'NONE',  ( -0.3000000000000161982, -114.9999999999982236, -0.9539392014169785217 ) ) ;
#2249 = CARTESIAN_POINT ( 'NONE',  ( -8.599996472200352571, -47.20000000000001705, 0.1525981975067654817 ) ) ;
#2250 = LINE ( 'NONE', #2716, #3222 ) ;
#2251 = ORIENTED_EDGE ( 'NONE', *, *, #2178, .T. ) ;
#2252 = DIRECTION ( 'NONE',  ( 0.000000000000000000, 1.000000000000000000, 0.000000000000000000 ) ) ;
#2253 = CARTESIAN_POINT ( 'NONE',  ( -11.39999532361432522, -52.79999999999999716, 0.1755699507458657049 ) ) ;
#2254 = DIRECTION ( 'NONE',  ( 0.000000000000000000, 0.000000000000000000, -1.000000000000000000 ) ) ;
#2255 = CARTESIAN_POINT ( 'NONE',  ( -0.3000000000000161982, -117.6667267801783225, -0.8135312584238875155 ) ) ;
#2256 = VECTOR ( 'NONE', #2348, 1000.000000000000000 ) ;
#2257 = CARTESIAN_POINT ( 'NONE',  ( 10.81682914263855544, -52.79999999999999716, 3.675996170187548540 ) ) ;
#2258 = VERTEX_POINT ( 'NONE', #254 ) ;
#2259 = CARTESIAN_POINT ( 'NONE',  ( 4.331939449206418047, -47.20000000000001705, 7.514224851275111305 ) ) ;
#2260 = EDGE_CURVE ( 'NONE', #3214, #342, #3031, .T. ) ;
#2261 = CARTESIAN_POINT ( 'NONE',  ( 1.836970198721029688E-16, -104.9999999999982379, -1.499999999999999778 ) ) ;
#2262 = CARTESIAN_POINT ( 'NONE',  ( -4.815279722017292485, -50.66710047508086490, -1.347079874192880444 ) ) ;
#2263 =( GEOMETRIC_REPRESENTATION_CONTEXT ( 3 ) GLOBAL_UNCERTAINTY_ASSIGNED_CONTEXT ( ( #1262 ) ) GLOBAL_UNIT_ASSIGNED_CONTEXT ( ( #132, #1669, #2394 ) ) REPRESENTATION_CONTEXT ( 'NONE', 'WORKASPACE' ) );
#2264 = ADVANCED_FACE ( 'NONE', ( #1296 ), #2325, .T. ) ;
#2265 = CARTESIAN_POINT ( 'NONE',  ( 6.124525076959063726E-16, 7.500000000000000000, -4.999999999999999112 ) ) ;
#2266 = CARTESIAN_POINT ( 'NONE',  ( -5.000000000000000000, 24.40983005625052726, 18.00000000000000355 ) ) ;
#2267 = CARTESIAN_POINT ( 'NONE',  ( 11.40000778997679198, -52.79999999999999716, -0.2924664341912773247 ) ) ;
#2268 = CARTESIAN_POINT ( 'NONE',  ( 4.985642101603771081, -48.54846037558075267, 0.3907762206522687465 ) ) ;
#2269 = CIRCLE ( 'NONE', #642, 4.999999999999998224 ) ;
#2270 = B_SPLINE_CURVE_WITH_KNOTS ( 'NONE', 3,
 ( #948, #724, #186, #1183, #1482, #2479, #1695, #2216, #1947, #3002, #474, #202 ),
 .UNSPECIFIED., .F., .F.,
 ( 4, 2, 2, 2, 2, 4 ),
 ( 0.002664946375549228936, 0.002999773306175310215, 0.003334600236801391060, 0.004004254098053570965, 0.004673907959305750003, 0.005343561820557929040 ),
 .UNSPECIFIED. ) ;
#2271 = CARTESIAN_POINT ( 'NONE',  ( 8.160064090060387798, -50.00000000000000000, 2.773119917860402239 ) ) ;
#2272 = EDGE_CURVE ( 'NONE', #1839, #2538, #1534, .T. ) ;
#2273 = ORIENTED_EDGE ( 'NONE', *, *, #1414, .T. ) ;
#2274 = AXIS2_PLACEMENT_3D ( 'NONE', #155, #932, #916 ) ;
#2275 = CARTESIAN_POINT ( 'NONE',  ( 2.108823893667861604, 7.199131270151879924, -4.536514892156152889 ) ) ;
#2276 = CONTEXT_DEPENDENT_SHAPE_REPRESENTATION ( #3045, #1650 ) ;
#2277 = CIRCLE ( 'NONE', #1743, 2.500000000000000444 ) ;
#2278 =( GEOMETRIC_REPRESENTATION_CONTEXT ( 3 ) GLOBAL_UNCERTAINTY_ASSIGNED_CONTEXT ( ( #2032 ) ) GLOBAL_UNIT_ASSIGNED_CONTEXT ( ( #382, #1904, #1390 ) ) REPRESENTATION_CONTEXT ( 'NONE', 'WORKASPACE' ) );
#2279 = DIRECTION ( 'NONE',  ( 0.000000000000000000, 0.000000000000000000, 1.000000000000000000 ) ) ;
#2280 =( GEOMETRIC_REPRESENTATION_CONTEXT ( 3 ) GLOBAL_UNCERTAINTY_ASSIGNED_CONTEXT ( ( #542 ) ) GLOBAL_UNIT_ASSIGNED_CONTEXT ( ( #1083, #1796, #2347 ) ) REPRESENTATION_CONTEXT ( 'NONE', 'WORKASPACE' ) );
#2281 = CARTESIAN_POINT ( 'NONE',  ( -2.499999999999999556, 0.000000000000000000, -10.00000000000000000 ) ) ;
#2282 = CYLINDRICAL_SURFACE ( 'NONE', #152, 7.500000000000000888 ) ;
#2283 = CARTESIAN_POINT ( 'NONE',  ( 0.000000000000000000, 0.000000000000000000, 10.00000000000000000 ) ) ;
#2284 = DIRECTION ( 'NONE',  ( 1.000000000000000000, 0.000000000000000000, 0.000000000000000000 ) ) ;
#2285 = CARTESIAN_POINT ( 'NONE',  ( 8.906419880262733457, -50.95872650893685574, 1.034857390322859061 ) ) ;
#2286 = CARTESIAN_POINT ( 'NONE',  ( 8.572276570257084671, -50.00000000000000000, 0.7042094815225934390 ) ) ;
#2287 = ORIENTED_EDGE ( 'NONE', *, *, #2030, .F. ) ;
#2288 = CARTESIAN_POINT ( 'NONE',  ( 0.000000000000000000, -72.60000000000000853, 2.300000000000000266 ) ) ;
#2289 = CARTESIAN_POINT ( 'NONE',  ( 0.000000000000000000, 0.000000000000000000, 18.00000000000000355 ) ) ;
#2290 = CARTESIAN_POINT ( 'NONE',  ( -7.500000000000000888, 30.00000000000000000, 10.00000000000000000 ) ) ;
#2291 = CYLINDRICAL_SURFACE ( 'NONE', #2161, 1.399999999999999911 ) ;
#2292 = ORIENTED_EDGE ( 'NONE', *, *, #136, .T. ) ;
#2293 = CARTESIAN_POINT ( 'NONE',  ( 4.784702204231576772, -50.39069709306253486, -1.451562066005745999 ) ) ;
#2294 = CARTESIAN_POINT ( 'NONE',  ( -4.999999999999999112, -66.68337520964460907, 0.000000000000000000 ) ) ;
#2295 = CARTESIAN_POINT ( 'NONE',  ( 0.000000000000000000, 80.00000000000000000, 4.999999999999999112 ) ) ;
#2296 = UNCERTAINTY_MEASURE_WITH_UNIT (LENGTH_MEASURE( 1.000000000000000082E-05 ), #2905, 'distance_accuracy_value', 'NONE');
#2297 = CARTESIAN_POINT ( 'NONE',  ( 0.000000000000000000, 30.00000000000000000, 18.00000000000000355 ) ) ;
#2298 = CARTESIAN_POINT ( 'NONE',  ( 3.061616997868383634E-16, -60.00000000000000000, 2.500000000000000444 ) ) ;
#2299 = DIRECTION ( 'NONE',  ( 1.000000000000000000, 0.000000000000000000, 0.000000000000000000 ) ) ;
#2300 = DIRECTION ( 'NONE',  ( 0.000000000000000000, -1.000000000000000000, 0.000000000000000000 ) ) ;
#2301 = CARTESIAN_POINT ( 'NONE',  ( 5.285102517541700351, -52.79999999999999716, 6.877134118846478295 ) ) ;
#2302 = ORIENTED_EDGE ( 'NONE', *, *, #1778, .T. ) ;
#2303 = CARTESIAN_POINT ( 'NONE',  ( -8.489369361306263073, -50.00000000000000000, 1.403517616197273554 ) ) ;
#2304 = CARTESIAN_POINT ( 'NONE',  ( -4.476439251420855747, -6.019721759973592157, 2.250752599798611975 ) ) ;
#2305 = ORIENTED_EDGE ( 'NONE', *, *, #553, .T. ) ;
#2306 = CARTESIAN_POINT ( 'NONE',  ( 2.499999999999999556, 3.061616997868382648E-16, -10.00000000000000000 ) ) ;
#2307 = APPLICATION_PROTOCOL_DEFINITION ( 'draft international standard', 'automotive_design', 1998, #1636 ) ;
#2308 = CARTESIAN_POINT ( 'NONE',  ( 8.596526774713710850, -47.20000000000001705, 0.2821220414049827041 ) ) ;
#2309 = AXIS2_PLACEMENT_3D ( 'NONE', #535, #782, #2550 ) ;
#2310 = ORIENTED_EDGE ( 'NONE', *, *, #306, .F. ) ;
#2311 = CARTESIAN_POINT ( 'NONE',  ( -3.790413940515794611, -74.65884673497926372, 3.275345238443577500 ) ) ;
#2312 = B_SPLINE_CURVE_WITH_KNOTS ( 'NONE', 3,
 ( #1168, #1463, #2694, #1709, #2725, #3252, #456, #2496, #2741, #218, #426, #2232, #2675, #3238, #1231, #2246, #2184, #979, #406, #1930, #2542, #524, #65, #1074, #82, #1091, #251, #851, #1528, #1834, #1510, #1259, #3017, #2018, #831, #2779, #756, #2522, #1745, #1499 ),
 .UNSPECIFIED., .F., .F.,
 ( 4, 2, 2, 2, 2, 2, 2, 2, 2, 2, 2, 2, 2, 2, 2, 2, 2, 2, 2, 4 ),
 ( 0.01615986362459447684, 0.01666419217584455895, 0.01716852072709463758, 0.01817717782959479833, 0.01918583493209496255, 0.02019449203459512329, 0.02120314913709528404, 0.02221180623959544478, 0.02271613479084552342, 0.02322046334209560553, 0.02422912044459576628, 0.02523777754709592702, 0.02574210609834600566, 0.02624643464959608777, 0.02725509175209624851, 0.02826374885459641273, 0.02927240595709657001, 0.03028106305959672728, 0.03128972016209689150, 0.03229837726459704877 ),
 .UNSPECIFIED. ) ;
#2313 = CARTESIAN_POINT ( 'NONE',  ( 8.572527594031472993E-15, -70.00000000000000000, 0.000000000000000000 ) ) ;
#2314 = MECHANICAL_DESIGN_GEOMETRIC_PRESENTATION_REPRESENTATION (  '', ( #2688 ), #2263 ) ;
#2315 = SHAPE_REPRESENTATION_RELATIONSHIP ( 'NONE' , 'NONE' ,  #1236, #617 ) ;
#2316 = CYLINDRICAL_SURFACE ( 'NONE', #1246, 1.500000000000000444 ) ;
#2317 = CARTESIAN_POINT ( 'NONE',  ( 8.596526774713712626, -50.00000000000000000, 0.2821220414049827596 ) ) ;
#2318 = ORIENTED_EDGE ( 'NONE', *, *, #751, .T. ) ;
#2319 = CARTESIAN_POINT ( 'NONE',  ( 8.599999999999996092, -50.00000000000000000, -1.093333333333372126 ) ) ;
#2320 = CARTESIAN_POINT ( 'NONE',  ( 6.000000000000010658, -70.00000000000000000, 10.00000000000000000 ) ) ;
#2321 = EDGE_LOOP ( 'NONE', ( #1931, #488, #1336, #380 ) ) ;
#2322 = CARTESIAN_POINT ( 'NONE',  ( 7.500000000000000000, 9.184850993605147944E-16, 10.00000000000000000 ) ) ;
#2323 = ADVANCED_FACE ( 'NONE', ( #1280 ), #25, .F. ) ;
#2324 = CARTESIAN_POINT ( 'NONE',  ( 2.982843918280841500, -47.20000000000001705, 11.10373667793903074 ) ) ;
#2325 = CONICAL_SURFACE ( 'NONE', #1687, 0.4999999999999813483, 0.04995839572193926104 ) ;
#2326 = EDGE_LOOP ( 'NONE', ( #1723, #628 ) ) ;
#2327 = CARTESIAN_POINT ( 'NONE',  ( -5.000012828558699773, -51.50004276186603391, 0.09784062508662537405 ) ) ;
#2328 = CIRCLE ( 'NONE', #1053, 7.500000000000000000 ) ;
#2329 = EDGE_CURVE ( 'NONE', #1564, #1865, #2010, .T. ) ;
#2330 = DIRECTION ( 'NONE',  ( 1.000000000000000000, 0.000000000000000000, 0.000000000000000000 ) ) ;
#2331 = ORIENTED_EDGE ( 'NONE', *, *, #234, .F. ) ;
#2332 = SURFACE_STYLE_USAGE ( .BOTH. , #256 ) ;
#2333 = CARTESIAN_POINT ( 'NONE',  ( -4.999999999999999112, 30.00000000000000000, 18.00000000000000355 ) ) ;
#2334 = CARTESIAN_POINT ( 'NONE',  ( 1.125736483477000061, -52.79999999999999716, 8.599999999999996092 ) ) ;
#2335 = EDGE_LOOP ( 'NONE', ( #1522, #1823 ) ) ;
#2336 = DIRECTION ( 'NONE',  ( 0.000000000000000000, 0.000000000000000000, 1.000000000000000000 ) ) ;
#2337 = PRESENTATION_STYLE_ASSIGNMENT (( #3092 ) ) ;
#2338 = CARTESIAN_POINT ( 'NONE',  ( 8.582665138674004268, -50.00000000000000000, 0.5636706063485154017 ) ) ;
#2339 = CARTESIAN_POINT ( 'NONE',  ( -1.331840593602624745, -7.388197954259797307, 4.830944097608436572 ) ) ;
#2340 = ORIENTED_EDGE ( 'NONE', *, *, #2617, .F. ) ;
#2341 = CARTESIAN_POINT ( 'NONE',  ( -3.320170879781855433, 6.729821324027721374, 3.751849819826997834 ) ) ;
#2342 = CARTESIAN_POINT ( 'NONE',  ( -7.513445500749801553, -47.20000000000001705, 4.333070140105379942 ) ) ;
#2343 = ORIENTED_EDGE ( 'NONE', *, *, #804, .F. ) ;
#2344 = DIRECTION ( 'NONE',  ( -0.000000000000000000, -1.000000000000000000, -0.000000000000000000 ) ) ;
#2345 = CARTESIAN_POINT ( 'NONE',  ( 0.1574018113688459009, -114.7330607081729568, 1.002653532495389577 ) ) ;
#2346 = ORIENTED_EDGE ( 'NONE', *, *, #1983, .T. ) ;
#2347 =( NAMED_UNIT ( * ) SI_UNIT ( $, .STERADIAN. ) SOLID_ANGLE_UNIT ( ) );
#2348 = DIRECTION ( 'NONE',  ( -0.000000000000000000, -1.000000000000000000, -0.000000000000000000 ) ) ;
#2349 = CARTESIAN_POINT ( 'NONE',  ( -8.596526774713707297, -50.00000000000000000, 0.2821220414048196679 ) ) ;
#2350 = ORIENTED_EDGE ( 'NONE', *, *, #3241, .F. ) ;
#2351 = DIRECTION ( 'NONE',  ( 0.000000000000000000, -1.000000000000000000, 0.000000000000000000 ) ) ;
#2352 = FILL_AREA_STYLE ('',( #1848 ) ) ;
#2353 = CARTESIAN_POINT ( 'NONE',  ( 1.654849718955805127, 7.321828482412975347, 4.729586325473386310 ) ) ;
#2354 = CARTESIAN_POINT ( 'NONE',  ( 1.836970198721029688E-16, -84.99999999999998579, -1.499999999999999778 ) ) ;
#2355 = CARTESIAN_POINT ( 'NONE',  ( -4.324727228821070746, -6.131211258369285488, 2.529220782163199122 ) ) ;
#2356 = ORIENTED_EDGE ( 'NONE', *, *, #2111, .T. ) ;
#2357 = CARTESIAN_POINT ( 'NONE',  ( -2.259265036967212481, 7.158401641891561695, 4.472413388026437175 ) ) ;
#2358 = CARTESIAN_POINT ( 'NONE',  ( -7.005833569763921354, -47.20000000000001705, 9.116201041262108618 ) ) ;
#2359 = ORIENTED_EDGE ( 'NONE', *, *, #3194, .F. ) ;
#2360 = CARTESIAN_POINT ( 'NONE',  ( -0.6584138513982479290, -72.41738593900605281, -4.959126935340800735 ) ) ;
#2361 = AXIS2_PLACEMENT_3D ( 'NONE', #3198, #1721, #1923 ) ;
#2362 = CARTESIAN_POINT ( 'NONE',  ( -8.485280282859317680, -50.00000000000000000, 1.400000000000003020 ) ) ;
#2363 = ORIENTED_EDGE ( 'NONE', *, *, #1312, .T. ) ;
#2364 = FACE_OUTER_BOUND ( 'NONE', #1871, .T. ) ;
#2365 = ADVANCED_FACE ( 'NONE', ( #288 ), #1762, .F. ) ;
#2366 = FACE_BOUND ( 'NONE', #658, .T. ) ;
#2367 = ORIENTED_EDGE ( 'NONE', *, *, #2059, .T. ) ;
#2368 = AXIS2_PLACEMENT_3D ( 'NONE', #578, #1616, #859 ) ;
#2369 = CYLINDRICAL_SURFACE ( 'NONE', #2791, 2.300000000000000266 ) ;
#2370 = AXIS2_PLACEMENT_3D ( 'NONE', #257, #1018, #2152 ) ;
#2371 = DIRECTION ( 'NONE',  ( -0.000000000000000000, -1.000000000000000000, -0.000000000000000000 ) ) ;
#2372 = DIRECTION ( 'NONE',  ( 0.000000000000000000, 0.000000000000000000, 1.000000000000000000 ) ) ;
#2373 = CARTESIAN_POINT ( 'NONE',  ( -4.733269301232542858, -5.819947390767942430, -1.643717648664120068 ) ) ;
#2374 = ORIENTED_EDGE ( 'NONE', *, *, #1391, .T. ) ;
#2375 = CARTESIAN_POINT ( 'NONE',  ( -3.971811635560102527, 6.365546751009641291, -3.053863045737025494 ) ) ;
#2376 = ADVANCED_FACE ( 'NONE', ( #1982 ), #1216, .F. ) ;
#2377 = CARTESIAN_POINT ( 'NONE',  ( -11.25335008359228794, -50.00000000000000000, 1.860476840075229621 ) ) ;
#2378 = VERTEX_POINT ( 'NONE', #2445 ) ;
#2379 = CARTESIAN_POINT ( 'NONE',  ( -8.485280282859317680, -50.00000000000000000, 1.400000000000003020 ) ) ;
#2380 = AXIS2_PLACEMENT_3D ( 'NONE', #638, #2637, #827 ) ;
#2381 = CARTESIAN_POINT ( 'NONE',  ( -2.347667281524951198E-13, -114.6999999999962228, 1.015000000000727765 ) ) ;
#2382 = EDGE_LOOP ( 'NONE', ( #323, #1994, #2027, #1061 ) ) ;
#2383 = CIRCLE ( 'NONE', #2795, 7.500000000000000888 ) ;
#2384 = DIRECTION ( 'NONE',  ( -0.000000000000000000, -0.000000000000000000, 1.000000000000000000 ) ) ;
#2385 =( BOUNDED_CURVE ( )  B_SPLINE_CURVE ( 3, ( #363, #2598, #1085, #2099 ),
 .UNSPECIFIED., .F., .T. ) 
 B_SPLINE_CURVE_WITH_KNOTS ( ( 4, 4 ),
 ( 0.000000000000000000, 1.570796326794896780 ),
 .UNSPECIFIED. ) 
 CURVE ( )  GEOMETRIC_REPRESENTATION_ITEM ( )  RATIONAL_B_SPLINE_CURVE ( ( 1.000000000000000000, 0.8047378541243649375, 0.8047378541243649375, 1.000000000000000000 ) ) 
 REPRESENTATION_ITEM ( '' )  );
#2386 = DIRECTION ( 'NONE',  ( -0.000000000000000000, -0.000000000000000000, 1.000000000000000000 ) ) ;
#2387 = CARTESIAN_POINT ( 'NONE',  ( 2.368690460745422222, -69.18407089167581603, -4.403897978979204986 ) ) ;
#2388 = EDGE_LOOP ( 'NONE', ( #550, #172, #3082, #1459, #1353 ) ) ;
#2389 = DIRECTION ( 'NONE',  ( 0.000000000000000000, 1.000000000000000000, 0.000000000000000000 ) ) ;
#2390 = DIRECTION ( 'NONE',  ( 0.000000000000000000, 0.000000000000000000, 1.000000000000000000 ) ) ;
#2391 = AXIS2_PLACEMENT_3D ( 'NONE', #1033, #2771, #2284 ) ;
#2392 = CARTESIAN_POINT ( 'NONE',  ( 0.3421168542193412376, 7.499999999999999112, 4.999999999999999112 ) ) ;
#2393 = CARTESIAN_POINT ( 'NONE',  ( -11.39999999999999680, -50.00000000000000000, -1.093333333333363022 ) ) ;
#2394 =( NAMED_UNIT ( * ) SI_UNIT ( $, .STERADIAN. ) SOLID_ANGLE_UNIT ( ) );
#2395 = CARTESIAN_POINT ( 'NONE',  ( -2.541265623391468331, 7.062137256042765543, 4.317949725309306430 ) ) ;
#2396 = CARTESIAN_POINT ( 'NONE',  ( 11.39999999999999680, -47.20000000000001705, -1.366666666666861873 ) ) ;
#2397 = ORIENTED_EDGE ( 'NONE', *, *, #1289, .F. ) ;
#2398 = PRODUCT_DEFINITION_SHAPE ( 'NONE', 'NONE',  #3278 ) ;
#2399 = CARTESIAN_POINT ( 'NONE',  ( -6.610444160707455418E-15, -72.50000000000009948, -5.000000000000047962 ) ) ;
#2400 = VERTEX_POINT ( 'NONE', #171 ) ;
#2401 = DIRECTION ( 'NONE',  ( -0.000000000000000000, -0.000000000000000000, 1.000000000000000000 ) ) ;
#2402 = PLANE ( 'NONE',  #2096 ) ;
#2403 = CARTESIAN_POINT ( 'NONE',  ( 0.6585099098572929632, -67.58258473628077923, -4.959140660327080674 ) ) ;
#2404 = ORIENTED_EDGE ( 'NONE', *, *, #2868, .T. ) ;
#2405 = FACE_OUTER_BOUND ( 'NONE', #1576, .T. ) ;
#2406 = SURFACE_STYLE_USAGE ( .BOTH. , #1406 ) ;
#2407 = CARTESIAN_POINT ( 'NONE',  ( -11.39999999999999680, -47.20000000000001705, -0.5466666666666361030 ) ) ;
#2408 = CARTESIAN_POINT ( 'NONE',  ( -4.999850703040199740, -5.590303478919644853, 0.1739517833579089512 ) ) ;
#2409 = DIRECTION ( 'NONE',  ( 0.000000000000000000, -0.000000000000000000, 1.000000000000000000 ) ) ;
#2410 = EDGE_CURVE ( 'NONE', #1696, #1290, #2270, .T. ) ;
#2411 = CARTESIAN_POINT ( 'NONE',  ( 11.39999999999999680, -50.00000000000000000, -1.093333333333372126 ) ) ;
#2412 = VERTEX_POINT ( 'NONE', #2198 ) ;
#2413 = DIRECTION ( 'NONE',  ( 1.000000000000000000, 0.000000000000000000, 0.000000000000000000 ) ) ;
#2414 = EDGE_CURVE ( 'NONE', #1054, #903, #2328, .T. ) ;
#2415 = ORIENTED_EDGE ( 'NONE', *, *, #1285, .F. ) ;
#2416 = CARTESIAN_POINT ( 'NONE',  ( -2.241708953382383296, -68.88112708827009101, -4.469887766052389466 ) ) ;
#2417 = EDGE_CURVE ( 'NONE', #2549, #2400, #644, .T. ) ;
#2418 = CARTESIAN_POINT ( 'NONE',  ( -8.599999999999996092, -50.00000000000000000, -1.093333333333363022 ) ) ;
#2419 = PLANE ( 'NONE',  #1159 ) ;
#2420 = ORIENTED_EDGE ( 'NONE', *, *, #1874, .T. ) ;
#2421 = CARTESIAN_POINT ( 'NONE',  ( 3.061616997868384127E-16, -72.50000000000001421, 2.500000000000000444 ) ) ;
#2422 = CLOSED_SHELL ( 'NONE', ( #710, #72, #2697, #2376, #1134, #1821, #2531, #1573, #1512, #2886, #2465, #2009, #2692, #1988, #213, #165, #609, #1130, #1879, #1715, #54, #105, #2365, #1739, #1373, #2892, #757, #22 ) ) ;
#2423 = CARTESIAN_POINT ( 'NONE',  ( 8.599999999999996092, -47.20000000000001705, -1.366666666666861873 ) ) ;
#2424 = CARTESIAN_POINT ( 'NONE',  ( -4.325873777034227707, -6.130418473463322471, -2.527359400829327196 ) ) ;
#2425 = DIRECTION ( 'NONE',  ( -0.000000000000000000, -0.000000000000000000, 1.000000000000000000 ) ) ;
#2426 = CARTESIAN_POINT ( 'NONE',  ( -10.81682914263834405, -50.00000000000000000, 3.675996170188739143 ) ) ;
#2427 = EDGE_LOOP ( 'NONE', ( #2363, #2146 ) ) ;
#2428 = FACE_OUTER_BOUND ( 'NONE', #2442, .T. ) ;
#2429 = DIRECTION ( 'NONE',  ( -0.000000000000000000, -0.000000000000000000, -1.000000000000000000 ) ) ;
#2430 = EDGE_LOOP ( 'NONE', ( #2397, #2415, #1766, #1597 ) ) ;
#2431 = AXIS2_PLACEMENT_3D ( 'NONE', #543, #1551, #2557 ) ;
#2432 = CARTESIAN_POINT ( 'NONE',  ( 8.599999999999996092, -50.00000000000000000, -1.366666666666861873 ) ) ;
#2433 = CARTESIAN_POINT ( 'NONE',  ( 8.767617449782822092, -49.18583174968845384, 1.157007882117269792 ) ) ;
#2434 = DIRECTION ( 'NONE',  ( 0.000000000000000000, 0.000000000000000000, -1.000000000000000000 ) ) ;
#2435 = AXIS2_PLACEMENT_3D ( 'NONE', #1432, #3188, #2459 ) ;
#2436 = CARTESIAN_POINT ( 'NONE',  ( -4.977300154039397739, -48.57702733233907821, 0.4847224211361968460 ) ) ;
#2437 = STYLED_ITEM ( 'NONE', ( #1867 ), #1401 ) ;
#2438 = CARTESIAN_POINT ( 'NONE',  ( 10.81682914263912210, -47.20000000000001705, 3.675996170187548540 ) ) ;
#2439 = PRESENTATION_LAYER_ASSIGNMENT (  '', '', ( #1645 ) ) ;
#2440 = CARTESIAN_POINT ( 'NONE',  ( -8.768448914935611072, -50.81504429929021427, 1.156277961913375618 ) ) ;
#2441 = CARTESIAN_POINT ( 'NONE',  ( -1.125736483477000061, -52.79999999999999716, 8.599999999999996092 ) ) ;
#2442 = EDGE_LOOP ( 'NONE', ( #1009, #2343, #1769, #2367 ) ) ;
#2443 = CARTESIAN_POINT ( 'NONE',  ( -8.160064090060583197, -47.20000000000001705, 2.773119917861301520 ) ) ;
#2444 = B_SPLINE_CURVE_WITH_KNOTS ( 'NONE', 3,
 ( #2242, #1426, #704, #3233, #974, #687, #1959, #3248, #2440, #1992, #2996, #2750, #1704, #1670 ),
 .UNSPECIFIED., .F., .F.,
 ( 4, 2, 2, 2, 2, 2, 4 ),
 ( -7.483321517452871261E-06, 0.0003315069634277711215, 0.0006704972483729951726, 0.001348477818263447937, 0.002026458388153901027, 0.002365448673099125945, 0.002704438958044351297 ),
 .UNSPECIFIED. ) ;
#2445 = CARTESIAN_POINT ( 'NONE',  ( -10.00000000000001776, -51.39999999999999858, 1.734719586992576771E-19 ) ) ;
#2446 = ORIENTED_EDGE ( 'NONE', *, *, #2213, .T. ) ;
#2447 = CARTESIAN_POINT ( 'NONE',  ( 0.000000000000000000, -80.00000000000000000, 4.999999999999999112 ) ) ;
#2448 = EDGE_CURVE ( 'NONE', #903, #1054, #1108, .T. ) ;
#2449 = CARTESIAN_POINT ( 'NONE',  ( 4.331939449206418935, -50.00000000000000000, 7.514224851275112194 ) ) ;
#2450 = CYLINDRICAL_SURFACE ( 'NONE', #2114, 7.500000000000000888 ) ;
#2451 = CARTESIAN_POINT ( 'NONE',  ( 1.375028959113674842, -75.85031115372576949, 4.819517586941451270 ) ) ;
#2452 = CARTESIAN_POINT ( 'NONE',  ( -4.945480083184111919, -48.69114140900990151, 0.7590239407556941265 ) ) ;
#2453 = CARTESIAN_POINT ( 'NONE',  ( 8.600005876649037262, -47.20000000000001705, -0.2541998246239300374 ) ) ;
#2454 = CARTESIAN_POINT ( 'NONE',  ( 4.769696007084725409, -49.90026769176149202, -1.500000000000006661 ) ) ;
#2455 = CARTESIAN_POINT ( 'NONE',  ( 0.000000000000000000, -104.9999999999982379, 0.000000000000000000 ) ) ;
#2456 = CARTESIAN_POINT ( 'NONE',  ( -8.599996472200352571, -52.79999999999999716, 0.1525981975067654817 ) ) ;
#2457 = ORIENTED_EDGE ( 'NONE', *, *, #482, .T. ) ;
#2458 = CARTESIAN_POINT ( 'NONE',  ( -5.285102517542626721, -50.00000000000000000, 6.877134118847252786 ) ) ;
#2459 = DIRECTION ( 'NONE',  ( 1.000000000000000000, 0.000000000000000000, 0.000000000000000000 ) ) ;
#2460 = EDGE_LOOP ( 'NONE', ( #1918, #753, #1242, #338, #409, #737, #2150, #893 ) ) ;
#2461 = CARTESIAN_POINT ( 'NONE',  ( 2.309991845038998903, -64.45292862506686049, 4.447043502685485983 ) ) ;
#2462 = CARTESIAN_POINT ( 'NONE',  ( 8.160064090060387798, -50.00000000000000000, 2.773119917860402239 ) ) ;
#2463 = CARTESIAN_POINT ( 'NONE',  ( 4.769696007084725409, -50.00000000000000000, -1.500000000000006439 ) ) ;
#2464 = CARTESIAN_POINT ( 'NONE',  ( 11.33527052789730050, -50.43454227690138225, -1.335270527897303827 ) ) ;
#2465 = ADVANCED_FACE ( 'NONE', ( #2971 ), #1661, .F. ) ;
#2466 = CARTESIAN_POINT ( 'NONE',  ( -4.769696007084727185, -49.80352985508882568, 1.499999999999993339 ) ) ;
#2467 =( BOUNDED_CURVE ( )  B_SPLINE_CURVE ( 3, ( #623, #2896, #2686, #1177 ),
 .UNSPECIFIED., .F., .F. ) 
 B_SPLINE_CURVE_WITH_KNOTS ( ( 4, 4 ),
 ( 1.570796326794896558, 3.141592653589794448 ),
 .UNSPECIFIED. ) 
 CURVE ( )  GEOMETRIC_REPRESENTATION_ITEM ( )  RATIONAL_B_SPLINE_CURVE ( ( 1.000000000000000000, 0.8047378541243646044, 0.8047378541243646044, 1.000000000000000000 ) ) 
 REPRESENTATION_ITEM ( '' )  );
#2468 = CARTESIAN_POINT ( 'NONE',  ( 1.492255338562904265, -52.79999999999999716, 11.39999999999999680 ) ) ;
#2469 = CARTESIAN_POINT ( 'NONE',  ( 4.815110478384604598, -49.33416175143172921, 1.347678760471933135 ) ) ;
#2470 = MECHANICAL_DESIGN_GEOMETRIC_PRESENTATION_REPRESENTATION (  '', ( #1622 ), #460 ) ;
#2471 = FACE_OUTER_BOUND ( 'NONE', #396, .T. ) ;
#2472 = CLOSED_SHELL ( 'NONE', ( #2928, #2323, #2247, #1495, #3141, #1913, #636, #978, #3258, #652, #2149, #2165, #280, #2855 ) ) ;
#2473 = ADVANCED_BREP_SHAPE_REPRESENTATION ( '', ( #491, #1692 ), #1537 ) ;
#2474 = CARTESIAN_POINT ( 'NONE',  ( 8.596526774713710850, -52.79999999999999716, 0.2821220414049827041 ) ) ;
#2475 = ORIENTED_EDGE ( 'NONE', *, *, #2848, .F. ) ;
#2476 = CIRCLE ( 'NONE', #3259, 7.500000000000000000 ) ;
#2477 = CARTESIAN_POINT ( 'NONE',  ( -8.596526774713705521, -47.20000000000001705, 0.2821220414048196123 ) ) ;
#2478 = FACE_OUTER_BOUND ( 'NONE', #2321, .T. ) ;
#2479 = CARTESIAN_POINT ( 'NONE',  ( 11.16040725319407123, -49.19031162998081896, -1.160407253194085220 ) ) ;
#2480 = ORIENTED_EDGE ( 'NONE', *, *, #36, .F. ) ;
#2481 = DIRECTION ( 'NONE',  ( 0.000000000000000000, 1.000000000000000000, 0.000000000000000000 ) ) ;
#2482 = CARTESIAN_POINT ( 'NONE',  ( -1.125736483476999839, -50.00000000000000000, 8.599999999999996092 ) ) ;
#2483 = CARTESIAN_POINT ( 'NONE',  ( 2.500000000000004441, -70.00000000000000000, 0.000000000000000000 ) ) ;
#2484 = CARTESIAN_POINT ( 'NONE',  ( 0.000000000000000000, -125.0000000000000000, 0.000000000000000000 ) ) ;
#2485 = DIRECTION ( 'NONE',  ( 0.000000000000000000, 0.000000000000000000, 1.000000000000000000 ) ) ;
#2486 = APPLICATION_CONTEXT ( 'automotive_design' ) ;
#2487 = CARTESIAN_POINT ( 'NONE',  ( -11.36325033731753287, -52.79999999999999716, 0.9334869871344718684 ) ) ;
#2488 = CIRCLE ( 'NONE', #2380, 2.300000000000000266 ) ;
#2489 = CARTESIAN_POINT ( 'NONE',  ( 11.39999999999999680, -50.00000000000000000, -1.400000000003877254 ) ) ;
#2490 = CARTESIAN_POINT ( 'NONE',  ( -10.15747651436539734, -51.39999999999999858, -0.1574726269690627789 ) ) ;
#2491 = ADVANCED_FACE ( 'NONE', ( #443 ), #1417, .F. ) ;
#2492 = CARTESIAN_POINT ( 'NONE',  ( 11.39999999999999680, -52.79999999999999716, -0.5466666666666269991 ) ) ;
#2493 = CIRCLE ( 'NONE', #1322, 4.999999999999999112 ) ;
#2494 = EDGE_LOOP ( 'NONE', ( #1448, #1012 ) ) ;
#2495 = CARTESIAN_POINT ( 'NONE',  ( -8.160064090060583197, -50.00000000000000000, 2.773119917861301964 ) ) ;
#2496 = CARTESIAN_POINT ( 'NONE',  ( 2.262527220957939456, -7.157552900320828471, -4.471083064257649120 ) ) ;
#2497 = CARTESIAN_POINT ( 'NONE',  ( 7.500000000000000888, 30.00000000000000000, 10.00000000000000000 ) ) ;
#2498 = CARTESIAN_POINT ( 'NONE',  ( -11.39999999999999680, -47.20000000000001705, -0.5466666666666361030 ) ) ;
#2499 = CARTESIAN_POINT ( 'NONE',  ( 6.123233995736765296E-16, 80.00000000000000000, -4.999999999999999112 ) ) ;
#2500 = CARTESIAN_POINT ( 'NONE',  ( 3.359434976081794311, -74.97862781767101126, 3.716172273690823147 ) ) ;
#2501 = CARTESIAN_POINT ( 'NONE',  ( 0.2999999999999837796, -114.9999999999982236, -0.9539392014169875145 ) ) ;
#2502 = CARTESIAN_POINT ( 'NONE',  ( 11.39999999999999680, -50.00000000000000000, -0.5466666666666269991 ) ) ;
#2503 = CARTESIAN_POINT ( 'NONE',  ( 4.916145513835878944, -48.80134495313303944, 0.9228047480949569392 ) ) ;
#2504 = CARTESIAN_POINT ( 'NONE',  ( 9.116201041288118034, -52.79999999999999716, 7.005833569791843907 ) ) ;
#2505 = ORIENTED_EDGE ( 'NONE', *, *, #925, .T. ) ;
#2506 = CARTESIAN_POINT ( 'NONE',  ( -8.530791689320901483, -47.20000000000001705, 1.124695299888049504 ) ) ;
#2507 = EDGE_CURVE ( 'NONE', #1865, #1564, #1427, .T. ) ;
#2508 = DIRECTION ( 'NONE',  ( -0.000000000000000000, 1.000000000000000000, -0.000000000000000000 ) ) ;
#2509 = CARTESIAN_POINT ( 'NONE',  ( 4.661216347248879899, -66.22080041675921791, 1.816027882404178229 ) ) ;
#2510 = EDGE_CURVE ( 'NONE', #1195, #1139, #2312, .T. ) ;
#2511 = ADVANCED_FACE ( 'NONE', ( #1757 ), #2842, .T. ) ;
#2512 = DIRECTION ( 'NONE',  ( -0.000000000000000000, -0.000000000000000000, 1.000000000000000000 ) ) ;
#2513 = DIRECTION ( 'NONE',  ( -0.000000000000000000, -0.000000000000000000, 1.000000000000000000 ) ) ;
#2514 = EDGE_CURVE ( 'NONE', #2870, #2171, #2904, .T. ) ;
#2515 = FACE_OUTER_BOUND ( 'NONE', #576, .T. ) ;
#2516 = CARTESIAN_POINT ( 'NONE',  ( 11.39999999999999680, -50.00000000000000000, -1.639999999999997460 ) ) ;
#2517 = CARTESIAN_POINT ( 'NONE',  ( 4.945591935980590215, -48.69073257577973379, 0.7581774313040230417 ) ) ;
#2518 = VECTOR ( 'NONE', #854, 1000.000000000000000 ) ;
#2519 = CARTESIAN_POINT ( 'NONE',  ( -8.160064090060583197, -50.00000000000000000, 2.773119917861301964 ) ) ;
#2520 = VERTEX_POINT ( 'NONE', #350 ) ;
#2521 = CARTESIAN_POINT ( 'NONE',  ( 0.000000000000000000, -84.99999999999998579, 0.000000000000000000 ) ) ;
#2522 = CARTESIAN_POINT ( 'NONE',  ( 0.6778607859896496057, -7.476644527972223564, 4.965157125901431101 ) ) ;
#2523 = CIRCLE ( 'NONE', #1095, 2.499999999999999556 ) ;
#2524 = CARTESIAN_POINT ( 'NONE',  ( -4.945591935980590215, -51.30926742422028752, 0.7581774313040230417 ) ) ;
#2525 = AXIS2_PLACEMENT_3D ( 'NONE', #1267, #1221, #808 ) ;
#2526 = CARTESIAN_POINT ( 'NONE',  ( -10.31385090661583526, -48.62614420630684009, -0.3138474430211326549 ) ) ;
#2527 = DIRECTION ( 'NONE',  ( 0.000000000000000000, 0.000000000000000000, 1.000000000000000000 ) ) ;
#2528 = DIRECTION ( 'NONE',  ( 1.000000000000000000, 0.000000000000000000, 0.000000000000000000 ) ) ;
#2529 = CARTESIAN_POINT ( 'NONE',  ( -8.599996472200352571, -52.79999999999999716, 0.1525981975067654817 ) ) ;
#2530 = ORIENTED_EDGE ( 'NONE', *, *, #161, .F. ) ;
#2531 = ADVANCED_FACE ( 'NONE', ( #503 ), #6, .T. ) ;
#2532 = SURFACE_STYLE_FILL_AREA ( #244 ) ;
#2533 = CARTESIAN_POINT ( 'NONE',  ( 2.500000000000008438, -70.16838717509892831, -4.330127018922188320 ) ) ;
#2534 = AXIS2_PLACEMENT_3D ( 'NONE', #1717, #1471, #2485 ) ;
#2535 = CYLINDRICAL_SURFACE ( 'NONE', #3156, 4.999999999999999112 ) ;
#2536 = PRODUCT_DEFINITION ( 'UNKNOWN', '', #594, #40 ) ;
#2537 = CARTESIAN_POINT ( 'NONE',  ( 4.331939449206418935, -50.00000000000000000, 7.514224851275112194 ) ) ;
#2538 = VERTEX_POINT ( 'NONE', #2261 ) ;
#2539 = AXIS2_PLACEMENT_3D ( 'NONE', #2769, #2429, #965 ) ;
#2540 = DIRECTION ( 'NONE',  ( -0.000000000000000000, 1.000000000000000000, -0.000000000000000000 ) ) ;
#2541 = MECHANICAL_DESIGN_GEOMETRIC_PRESENTATION_REPRESENTATION (  '', ( #590 ), #375 ) ;
#2542 = CARTESIAN_POINT ( 'NONE',  ( 5.000232060827701552, -5.589962382322530843, -0.3381422036129833608 ) ) ;
#2543 = DIRECTION ( 'NONE',  ( 0.000000000000000000, -0.000000000000000000, -1.000000000000000000 ) ) ;
#2544 = DIRECTION ( 'NONE',  ( 6.115594274737998660E-18, 0.9987523388778448696, -0.04993761694388874905 ) ) ;
#2545 = LINE ( 'NONE', #41, #1516 ) ;
#2546 = DIRECTION ( 'NONE',  ( 0.000000000000000000, 0.000000000000000000, 1.000000000000000000 ) ) ;
#2547 = FACE_OUTER_BOUND ( 'NONE', #1068, .T. ) ;
#2548 = CARTESIAN_POINT ( 'NONE',  ( 8.599996472200352571, -52.79999999999999716, 0.1525981975067867147 ) ) ;
#2549 = VERTEX_POINT ( 'NONE', #2294 ) ;
#2550 = DIRECTION ( 'NONE',  ( -1.000000000000000000, 0.000000000000000000, 0.000000000000000000 ) ) ;
#2551 = CARTESIAN_POINT ( 'NONE',  ( -2.258341722794894313, -7.158742388247099520, 4.472964013438597952 ) ) ;
#2552 = ORIENTED_EDGE ( 'NONE', *, *, #2852, .F. ) ;
#2553 = CYLINDRICAL_SURFACE ( 'NONE', #1299, 2.300000000000000266 ) ;
#2554 = CARTESIAN_POINT ( 'NONE',  ( -10.81682914263834405, -47.20000000000001705, 3.675996170188739143 ) ) ;
#2555 = CYLINDRICAL_SURFACE ( 'NONE', #2647, 2.499999999999999556 ) ;
#2556 = PRODUCT_DEFINITION_CONTEXT ( 'detailed design', #215, 'design' ) ;
#2557 = DIRECTION ( 'NONE',  ( 0.000000000000000000, 0.000000000000000000, -1.000000000000000000 ) ) ;
#2558 = FACE_OUTER_BOUND ( 'NONE', #2816, .T. ) ;
#2559 = CARTESIAN_POINT ( 'NONE',  ( 9.677496024927361162, -51.36581032562466476, 0.3176491571778780054 ) ) ;
#2560 = CARTESIAN_POINT ( 'NONE',  ( 6.877134118866902845, -50.00000000000000000, 5.285102517562147995 ) ) ;
#2561 = ORIENTED_EDGE ( 'NONE', *, *, #1289, .T. ) ;
#2562 = EDGE_CURVE ( 'NONE', #2549, #3219, #2587, .T. ) ;
#2563 = CARTESIAN_POINT ( 'NONE',  ( -0.3000000000000161982, -114.9999999999982236, -0.9539392014169785217 ) ) ;
#2564 = CARTESIAN_POINT ( 'NONE',  ( -8.324422814933019055, -50.00000000000000000, 2.231815450536601464 ) ) ;
#2565 = ORIENTED_EDGE ( 'NONE', *, *, #995, .F. ) ;
#2566 = CARTESIAN_POINT ( 'NONE',  ( 4.856197996442241482, -50.91599292333928872, 1.191843005749488871 ) ) ;
#2567 = CARTESIAN_POINT ( 'NONE',  ( 5.742338339643197287, -47.20000000000001705, 9.960716663318304853 ) ) ;
#2568 = B_SPLINE_CURVE_WITH_KNOTS ( 'NONE', 3,
 ( #208, #494, #1222, #160, #2238, #971, #1987, #1173, #2991, #2500, #921, #1935, #2940, #432, #2451, #2717, #177, #1188, #448, #805 ),
 .UNSPECIFIED., .F., .F.,
 ( 4, 2, 2, 2, 2, 2, 2, 2, 2, 4 ),
 ( 0.000000000000000000, 0.001046161093956322419, 0.002092322187912644838, 0.003138483281868968341, 0.004184644375825291411, 0.005230805469781614481, 0.006276966563737938418, 0.007323127657694261487, 0.007846208204672419986, 0.008369288751650577618 ),
 .UNSPECIFIED. ) ;
#2569 = CIRCLE ( 'NONE', #408, 1.499999999999999778 ) ;
#2570 = ORIENTED_EDGE ( 'NONE', *, *, #1175, .T. ) ;
#2571 = CARTESIAN_POINT ( 'NONE',  ( -4.815265823182749649, -73.58047044739645060, 1.356348383020188786 ) ) ;
#2572 = AXIS2_PLACEMENT_3D ( 'NONE', #1563, #1281, #2770 ) ;
#2573 = DIRECTION ( 'NONE',  ( 1.000000000000000000, 0.000000000000000000, -0.000000000000000000 ) ) ;
#2574 = VERTEX_POINT ( 'NONE', #2354 ) ;
#2575 = VECTOR ( 'NONE', #1069, 1000.000000000000000 ) ;
#2576 = DIRECTION ( 'NONE',  ( 0.000000000000000000, 0.000000000000000000, 1.000000000000000000 ) ) ;
#2577 = CARTESIAN_POINT ( 'NONE',  ( -11.39999999999999680, -50.00000000000000000, -1.400000000000000133 ) ) ;
#2578 = CARTESIAN_POINT ( 'NONE',  ( 2.250215587473118450, -52.79999999999999716, 8.376503107919017310 ) ) ;
#2579 = ORIENTED_EDGE ( 'NONE', *, *, #2912, .T. ) ;
#2580 = CARTESIAN_POINT ( 'NONE',  ( 0.000000000000000000, -60.00000000000000000, 0.000000000000000000 ) ) ;
#2581 = SHAPE_REPRESENTATION_RELATIONSHIP ( 'NONE' , 'NONE' ,  #457, #3218 ) ;
#2582 = CARTESIAN_POINT ( 'NONE',  ( 8.530791689320604831, -50.00000000000000000, 1.124695299888175182 ) ) ;
#2583 = CARTESIAN_POINT ( 'NONE',  ( -0.3421168542193412376, -7.499999999999999112, 4.999999999999999112 ) ) ;
#2584 = ORIENTED_EDGE ( 'NONE', *, *, #731, .F. ) ;
#2585 = DIRECTION ( 'NONE',  ( 0.000000000000000000, 0.000000000000000000, 1.000000000000000000 ) ) ;
#2586 = AXIS2_PLACEMENT_3D ( 'NONE', #3195, #209, #2703 ) ;
#2587 = B_SPLINE_CURVE_WITH_KNOTS ( 'NONE', 3,
 ( #1014, #2127, #1358, #3029, #1772, #233, #269, #490, #1278, #3095, #1245, #587, #1591, #998, #333, #2863, #2605, #101, #2107, #1339 ),
 .UNSPECIFIED., .F., .F.,
 ( 4, 2, 2, 2, 2, 2, 2, 2, 2, 4 ),
 ( 0.000000000000000000, 0.001046161093956322419, 0.002092322187912644404, 0.003138483281868967040, 0.004184644375825288809, 0.005230805469781612746, 0.006276966563737934948, 0.007323127657694257150, 0.007846208204672414782, 0.008369288751650572414 ),
 .UNSPECIFIED. ) ;
#2588 = EDGE_CURVE ( 'NONE', #1748, #123, #3114, .T. ) ;
#2589 = CARTESIAN_POINT ( 'NONE',  ( -8.599999999999996092, -47.20000000000001705, -0.5466666666666361030 ) ) ;
#2590 = AXIS2_PLACEMENT_3D ( 'NONE', #595, #1331, #2413 ) ;
#2591 = ORIENTED_EDGE ( 'NONE', *, *, #1898, .T. ) ;
#2592 = CARTESIAN_POINT ( 'NONE',  ( -4.772817378855775949, -50.19781530912092649, 1.490176662683681652 ) ) ;
#2593 = AXIS2_PLACEMENT_3D ( 'NONE', #1415, #723, #915 ) ;
#2594 = CARTESIAN_POINT ( 'NONE',  ( 0.2671601197814508222, -114.8429732948149109, 0.9734511544928151627 ) ) ;
#2595 = ORIENTED_EDGE ( 'NONE', *, *, #1189, .F. ) ;
#2596 = VECTOR ( 'NONE', #1182, 1000.000000000000000 ) ;
#2597 = DIRECTION ( 'NONE',  ( 1.000000000000000000, 0.000000000000000000, 0.000000000000000000 ) ) ;
#2598 = CARTESIAN_POINT ( 'NONE',  ( 1.464466094067265800, -72.50000000000001421, 2.499999999999999556 ) ) ;
#2599 = CARTESIAN_POINT ( 'NONE',  ( -8.599999999999996092, -50.00000000000000000, -1.366666666666159768 ) ) ;
#2600 = EDGE_LOOP ( 'NONE', ( #1693, #3235, #1600, #2287, #665 ) ) ;
#2601 = B_SPLINE_CURVE_WITH_KNOTS ( 'NONE', 3,
 ( #767, #3079, #1804, #501, #1820, #1755 ),
 .UNSPECIFIED., .F., .F.,
 ( 4, 2, 4 ),
 ( 1.973209580753283113E-07, 0.0002370058433632398788, 0.0004738143657684043076 ),
 .UNSPECIFIED. ) ;
#2602 = DIRECTION ( 'NONE',  ( 0.000000000000000000, 1.000000000000000000, 0.000000000000000000 ) ) ;
#2603 = SURFACE_STYLE_FILL_AREA ( #2352 ) ;
#2604 = CARTESIAN_POINT ( 'NONE',  ( 4.829496642845706234, 5.738802261244866365, 1.336683695250854953 ) ) ;
#2605 = CARTESIAN_POINT ( 'NONE',  ( -0.6967678811844660869, -64.03802537814742379, 4.954315763534758332 ) ) ;
#2606 = CARTESIAN_POINT ( 'NONE',  ( -3.971188403759415397, -6.365899760466498414, 3.054486213830300390 ) ) ;
#2607 = ORIENTED_EDGE ( 'NONE', *, *, #2507, .F. ) ;
#2608 = B_SPLINE_CURVE_WITH_KNOTS ( 'NONE', 3,
 ( #1667, #2466, #701, #1190, #938, #2718, #416, #2924, #2452, #2436, #465, #1920, #2204, #666, #162, #1174, #192, #2190, #2941, #684, #2222, #434, #1439, #3229, #957, #1974, #449, #178 ),
 .UNSPECIFIED., .F., .F.,
 ( 4, 2, 2, 2, 2, 2, 2, 2, 2, 2, 2, 2, 2, 4 ),
 ( 0.004716923349278730540, 0.005306377133062306975, 0.005601104024954096060, 0.005895830916845884277, 0.006485284700629445967, 0.006780011592521222909, 0.007074738484412999850, 0.007369465376304777660, 0.007664192268196553734, 0.008253646051980109352, 0.008548372943871894100, 0.008843099835763678848, 0.009137826727655463596, 0.009432553619547248344 ),
 .UNSPECIFIED. ) ;
#2609 = CARTESIAN_POINT ( 'NONE',  ( -4.722607672194940598, 5.826754641390677669, 1.650547109183062355 ) ) ;
#2610 = CARTESIAN_POINT ( 'NONE',  ( 8.599999999999996092, -47.20000000000001705, -1.639999999999997460 ) ) ;
#2611 = VERTEX_POINT ( 'NONE', #604 ) ;
#2612 = EDGE_CURVE ( 'NONE', #2199, #2182, #1608, .T. ) ;
#2613 = LINE ( 'NONE', #2901, #2063 ) ;
#2614 = CARTESIAN_POINT ( 'NONE',  ( 0.07907397510870638191, -114.6999999999981412, 1.015000000000068514 ) ) ;
#2615 = ORIENTED_EDGE ( 'NONE', *, *, #2999, .T. ) ;
#2616 = CARTESIAN_POINT ( 'NONE',  ( -0.6589706823815268955, -67.58264602806174537, -4.959110006177418484 ) ) ;
#2617 = EDGE_CURVE ( 'NONE', #2083, #2753, #1518, .T. ) ;
#2618 = LINE ( 'NONE', #1334, #2575 ) ;
#2619 = CARTESIAN_POINT ( 'NONE',  ( -6.877134118866000456, -50.00000000000000000, 5.285102517561346858 ) ) ;
#2620 = ORIENTED_EDGE ( 'NONE', *, *, #1330, .T. ) ;
#2621 = DIRECTION ( 'NONE',  ( 0.000000000000000000, 0.000000000000000000, -1.000000000000000000 ) ) ;
#2622 =( LENGTH_UNIT ( ) NAMED_UNIT ( * ) SI_UNIT ( .MILLI., .METRE. ) );
#2623 = CARTESIAN_POINT ( 'NONE',  ( 3.061616997868383634E-16, -60.00000000000000000, 2.500000000000000444 ) ) ;
#2624 = CARTESIAN_POINT ( 'NONE',  ( -2.499999999999999556, 3.061616997868382648E-16, 18.00000000000000355 ) ) ;
#2625 = CARTESIAN_POINT ( 'NONE',  ( -2.543753134549881167, -7.057059595574596500, -4.307653715470421751 ) ) ;
#2626 = EDGE_LOOP ( 'NONE', ( #1478, #1041, #2726, #2050, #2690 ) ) ;
#2627 = FACE_OUTER_BOUND ( 'NONE', #806, .T. ) ;
#2628 = CARTESIAN_POINT ( 'NONE',  ( -9.959683570761574956, -50.00000000000000000, 5.743837162464267898 ) ) ;
#2629 = CARTESIAN_POINT ( 'NONE',  ( -1.120846245543385855, -72.24071170040616607, -4.875204307872176734 ) ) ;
#2630 = CARTESIAN_POINT ( 'NONE',  ( 0.000000000000000000, 0.000000000000000000, 10.00000000000000000 ) ) ;
#2631 = EDGE_LOOP ( 'NONE', ( #346, #2042 ) ) ;
#2632 = PRODUCT_DEFINITION_SHAPE ( 'NONE', 'NONE',  #776 ) ;
#2633 = B_SPLINE_CURVE_WITH_KNOTS ( 'NONE', 3,
 ( #2399, #2644, #840, #2360, #3155, #2629, #1840, #1598, #2135, #1912, #902, #646, #2918, #89, #1647, #358 ),
 .UNSPECIFIED., .F., .F.,
 ( 4, 2, 2, 2, 2, 2, 2, 4 ),
 ( 0.003977372743944438890, 0.004474137685135931054, 0.004970902626327423218, 0.005467667567518916250, 0.005964432508710407546, 0.006957962391093391874, 0.007454727332284884038, 0.007951492273476376202 ),
 .UNSPECIFIED. ) ;
#2634 = CARTESIAN_POINT ( 'NONE',  ( 0.2999999999999999889, -114.9999999999982236, -2.300000000000000266 ) ) ;
#2635 = CARTESIAN_POINT ( 'NONE',  ( -0.3000000000000161982, -118.9999999999982379, 0.7416198487096099523 ) ) ;
#2636 = ORIENTED_EDGE ( 'NONE', *, *, #697, .F. ) ;
#2637 = DIRECTION ( 'NONE',  ( 0.000000000000000000, -1.000000000000000000, 0.000000000000000000 ) ) ;
#2638 = CARTESIAN_POINT ( 'NONE',  ( 1.331840593602624745, 7.388197954259797307, 4.830944097608436572 ) ) ;
#2639 = CARTESIAN_POINT ( 'NONE',  ( -11.30825875096015665, -47.20000000000001705, 1.490875164968288979 ) ) ;
#2640 = CARTESIAN_POINT ( 'NONE',  ( -3.769434200324356166, -6.488926209160664094, -3.300387065219955840 ) ) ;
#2641 = CARTESIAN_POINT ( 'NONE',  ( -3.326284669807233918, 6.726800191391157924, -3.746459129603366467 ) ) ;
#2642 = CARTESIAN_POINT ( 'NONE',  ( -11.36325033731753287, -52.79999999999999716, 0.9334869871344718684 ) ) ;
#2643 = ORIENTED_EDGE ( 'NONE', *, *, #2213, .F. ) ;
#2644 = CARTESIAN_POINT ( 'NONE',  ( -0.1665494872612699462, -72.50000000000004263, -5.000000000000003553 ) ) ;
#2645 = CIRCLE ( 'NONE', #205, 4.999999999999999112 ) ;
#2646 = EDGE_LOOP ( 'NONE', ( #2098, #2591, #3244, #2305 ) ) ;
#2647 = AXIS2_PLACEMENT_3D ( 'NONE', #252, #1760, #561 ) ;
#2648 = CARTESIAN_POINT ( 'NONE',  ( -1.880783153433909227, -68.34517127307829298, -4.634372473166646245 ) ) ;
#2649 = CARTESIAN_POINT ( 'NONE',  ( 7.500000000000000000, 9.184850993605147944E-16, -10.00000000000000000 ) ) ;
#2650 = DIRECTION ( 'NONE',  ( -0.000000000000000000, -0.000000000000000000, 1.000000000000000000 ) ) ;
#2651 =( GEOMETRIC_REPRESENTATION_CONTEXT ( 3 ) GLOBAL_UNCERTAINTY_ASSIGNED_CONTEXT ( ( #1761 ) ) GLOBAL_UNIT_ASSIGNED_CONTEXT ( ( #2666, #3148, #2817 ) ) REPRESENTATION_CONTEXT ( 'NONE', 'WORKASPACE' ) );
#2652 = ORIENTED_EDGE ( 'NONE', *, *, #1483, .F. ) ;
#2653 = FACE_OUTER_BOUND ( 'NONE', #2185, .T. ) ;
#2654 = CARTESIAN_POINT ( 'NONE',  ( -11.39999999999999680, -50.00000000000000000, -1.639999999999997460 ) ) ;
#2655 = CARTESIAN_POINT ( 'NONE',  ( -11.30825875096001454, -50.00000000000000000, 1.490875164968288757 ) ) ;
#2656 = CARTESIAN_POINT ( 'NONE',  ( -1.334319281011194347, 7.387780498848168342, 4.830307711356911504 ) ) ;
#2657 = EDGE_CURVE ( 'NONE', #2923, #1382, #1875, .T. ) ;
#2658 = CARTESIAN_POINT ( 'NONE',  ( -11.25335008359243005, -52.79999999999999716, 1.860476840075229843 ) ) ;
#2659 = EDGE_LOOP ( 'NONE', ( #567, #2140, #1257, #560 ) ) ;
#2660 = DIRECTION ( 'NONE',  ( 1.000000000000000000, 0.000000000000000000, 0.000000000000000000 ) ) ;
#2661 = ORIENTED_EDGE ( 'NONE', *, *, #731, .T. ) ;
#2662 = CARTESIAN_POINT ( 'NONE',  ( -7.513445500749800665, -50.00000000000000000, 4.333070140105378165 ) ) ;
#2663 = DIRECTION ( 'NONE',  ( 0.000000000000000000, 1.000000000000000000, 0.000000000000000000 ) ) ;
#2664 = EDGE_LOOP ( 'NONE', ( #376, #1610, #928, #3200 ) ) ;
#2665 = CARTESIAN_POINT ( 'NONE',  ( -2.499999999999995559, -71.46446609406727646, 1.464466094067262025 ) ) ;
#2666 =( LENGTH_UNIT ( ) NAMED_UNIT ( * ) SI_UNIT ( .MILLI., .METRE. ) );
#2667 = EDGE_CURVE ( 'NONE', #2258, #2713, #219, .T. ) ;
#2668 = CARTESIAN_POINT ( 'NONE',  ( -11.39999999999999680, -47.20000000000001705, -1.093333333333363022 ) ) ;
#2669 = CARTESIAN_POINT ( 'NONE',  ( -9.959683570761574956, -50.00000000000000000, 5.743837162464267898 ) ) ;
#2670 = MANIFOLD_SOLID_BREP ( 'Cut-Extrude2', #2422 ) ;
#2671 = CARTESIAN_POINT ( 'NONE',  ( -2.547727811071581527, 7.059815111224851947, -4.314169979798982091 ) ) ;
#2672 = CARTESIAN_POINT ( 'NONE',  ( 11.39999999999999680, -47.20000000000001705, -0.5466666666666269991 ) ) ;
#2673 = ORIENTED_EDGE ( 'NONE', *, *, #303, .F. ) ;
#2674 = CARTESIAN_POINT ( 'NONE',  ( -9.595856219366988071, -48.65479562300421179, 0.3963015081148661412 ) ) ;
#2675 = CARTESIAN_POINT ( 'NONE',  ( 3.971811635560102527, -6.365546751009641291, -3.053863045737025494 ) ) ;
#2676 = ORIENTED_EDGE ( 'NONE', *, *, #1533, .F. ) ;
#2677 = CARTESIAN_POINT ( 'NONE',  ( -2.164506549894624321, -68.73869660040230656, -4.508290309894544379 ) ) ;
#2678 = VECTOR ( 'NONE', #1025, 1000.000000000000000 ) ;
#2679 = CARTESIAN_POINT ( 'NONE',  ( 8.599999999999996092, -50.00000000000000000, -0.5466666666666269991 ) ) ;
#2680 = CARTESIAN_POINT ( 'NONE',  ( 3.061616997868383634E-16, -80.00000000000000000, 2.500000000000000444 ) ) ;
#2681 = ORIENTED_EDGE ( 'NONE', *, *, #952, .T. ) ;
#2682 = AXIS2_PLACEMENT_3D ( 'NONE', #486, #2336, #1072 ) ;
#2683 = CARTESIAN_POINT ( 'NONE',  ( 8.572527594031472993E-15, -70.00000000000000000, 0.000000000000000000 ) ) ;
#2684 = AXIS2_PLACEMENT_3D ( 'NONE', #790, #1315, #2330 ) ;
#2685 = CARTESIAN_POINT ( 'NONE',  ( 11.39999999999999680, -47.20000000000001705, -1.639999999999997460 ) ) ;
#2686 = CARTESIAN_POINT ( 'NONE',  ( 1.464466094067265356, -67.50000000000000000, 2.500000000000001332 ) ) ;
#2687 = CYLINDRICAL_SURFACE ( 'NONE', #138, 7.500000000000000888 ) ;
#2688=STYLED_ITEM('',(#3300),#491);
#2689 = CARTESIAN_POINT ( 'NONE',  ( -11.39999999999999680, -50.00000000000000000, -1.093333333333363022 ) ) ;
#2690 = ORIENTED_EDGE ( 'NONE', *, *, #1718, .T. ) ;
#2691 = CARTESIAN_POINT ( 'NONE',  ( -8.599999999999996092, -47.20000000000001705, -1.093333333333363022 ) ) ;
#2692 = ADVANCED_FACE ( 'NONE', ( #2364, #1843 ), #1663, .T. ) ;
#2693 = DIRECTION ( 'NONE',  ( -0.000000000000000000, -0.000000000000000000, 1.000000000000000000 ) ) ;
#2694 = CARTESIAN_POINT ( 'NONE',  ( 0.3368283383274193743, -7.494339828221662003, -4.991522157455978714 ) ) ;
#2695 = ORIENTED_EDGE ( 'NONE', *, *, #2081, .T. ) ;
#2696 = CARTESIAN_POINT ( 'NONE',  ( 4.858119196087237412, -66.47831555726492070, 1.194558663167264667 ) ) ;
#2697 = ADVANCED_FACE ( 'NONE', ( #1170 ), #1633, .F. ) ;
#2698 = VECTOR ( 'NONE', #2389, 1000.000000000000000 ) ;
#2699 = DIRECTION ( 'NONE',  ( 0.000000000000000000, 0.000000000000000000, 1.000000000000000000 ) ) ;
#2700 = CARTESIAN_POINT ( 'NONE',  ( -11.38641147205292192, -49.77694418854824221, -1.386411472052925697 ) ) ;
#2701 = CARTESIAN_POINT ( 'NONE',  ( -7.500000000000000000, -50.00000000000000000, -6.123233995736766085E-15 ) ) ;
#2702 = AXIS2_PLACEMENT_3D ( 'NONE', #2186, #2384, #112 ) ;
#2703 = DIRECTION ( 'NONE',  ( 0.000000000000000000, -0.000000000000000000, -1.000000000000000000 ) ) ;
#2704 = CARTESIAN_POINT ( 'NONE',  ( 5.742338339643197287, -47.20000000000001705, 9.960716663318304853 ) ) ;
#2705 = CARTESIAN_POINT ( 'NONE',  ( -0.3000000000000000444, -114.9201045547227977, 0.9581268606072530503 ) ) ;
#2706 = FACE_OUTER_BOUND ( 'NONE', #563, .T. ) ;
#2707 = CARTESIAN_POINT ( 'NONE',  ( 8.489369361306732031, -52.79999999999999716, 1.403517616196621409 ) ) ;
#2708 = VERTEX_POINT ( 'NONE', #1122 ) ;
#2709 = CARTESIAN_POINT ( 'NONE',  ( -8.599996472200352571, -50.00000000000000000, 0.1525981975067654262 ) ) ;
#2710 =( NAMED_UNIT ( * ) PLANE_ANGLE_UNIT ( ) SI_UNIT ( $, .RADIAN. ) );
#2711 = DIRECTION ( 'NONE',  ( 1.000000000000000000, 0.000000000000000000, 0.000000000000000000 ) ) ;
#2712 = EDGE_CURVE ( 'NONE', #694, #2708, #2137, .T. ) ;
#2713 = VERTEX_POINT ( 'NONE', #3143 ) ;
#2714 = CARTESIAN_POINT ( 'NONE',  ( 4.927416625552392127, -66.57594555594933183, 0.8653657731671272613 ) ) ;
#2715 = CARTESIAN_POINT ( 'NONE',  ( -4.999999999999999112, -80.00000000000000000, 0.000000000000000000 ) ) ;
#2716 = CARTESIAN_POINT ( 'NONE',  ( 0.000000000000000000, -60.00000000000000000, -2.500000000000000444 ) ) ;
#2717 = CARTESIAN_POINT ( 'NONE',  ( 0.8700260635408564314, -75.93904587936579276, 4.926729975457290855 ) ) ;
#2718 = CARTESIAN_POINT ( 'NONE',  ( -4.856197996442241482, -49.08400707666071128, 1.191843005749488871 ) ) ;
#2719 = CARTESIAN_POINT ( 'NONE',  ( -2.982843918280285944, -52.79999999999999716, 11.10373667793902541 ) ) ;
#2720 = CARTESIAN_POINT ( 'NONE',  ( 4.772817378855775949, -49.80218469087910904, 1.490176662683681652 ) ) ;
#2721 = LINE ( 'NONE', #1410, #1566 ) ;
#2722 = CARTESIAN_POINT ( 'NONE',  ( 8.530791689320606608, -52.79999999999999716, 1.124695299888175182 ) ) ;
#2723 = ORIENTED_EDGE ( 'NONE', *, *, #558, .T. ) ;
#2724 = CARTESIAN_POINT ( 'NONE',  ( -8.599999999999996092, -47.20000000000001705, -1.639999999999997460 ) ) ;
#2725 = CARTESIAN_POINT ( 'NONE',  ( 0.8431454290909620175, -7.454306392314355989, -4.931260737871609123 ) ) ;
#2726 = ORIENTED_EDGE ( 'NONE', *, *, #386, .T. ) ;
#2727 = CARTESIAN_POINT ( 'NONE',  ( 0.000000000000000000, 0.000000000000000000, 10.00000000000000000 ) ) ;
#2728 = CARTESIAN_POINT ( 'NONE',  ( -8.572276570256935457, -50.00000000000000000, 0.7042094815226510596 ) ) ;
#2729 = CARTESIAN_POINT ( 'NONE',  ( 7.500000000000000000, 9.184850993605147944E-16, 18.00000000000000355 ) ) ;
#2730 = ORIENTED_EDGE ( 'NONE', *, *, #2147, .F. ) ;
#2731 = DIRECTION ( 'NONE',  ( -0.000000000000000000, -0.000000000000000000, -1.000000000000000000 ) ) ;
#2732 = ADVANCED_FACE ( 'NONE', ( #2888 ), #712, .T. ) ;
#2733 = CARTESIAN_POINT ( 'NONE',  ( 9.116201041287551377, -50.00000000000000000, 7.005833569791843018 ) ) ;
#2734 = CARTESIAN_POINT ( 'NONE',  ( 4.772823807329270807, -49.80232464501099088, -1.490153625805560322 ) ) ;
#2735 = CARTESIAN_POINT ( 'NONE',  ( -10.31604092329497924, -51.37342103705936580, -0.3160374682705707761 ) ) ;
#2736 = CARTESIAN_POINT ( 'NONE',  ( -8.530791689320901483, -52.79999999999999716, 1.124695299888049504 ) ) ;
#2737 = ORIENTED_EDGE ( 'NONE', *, *, #3122, .F. ) ;
#2738 = CIRCLE ( 'NONE', #1825, 2.300000000000000266 ) ;
#2739 = CARTESIAN_POINT ( 'NONE',  ( -4.331939449206426929, -47.20000000000001705, 7.514224851276242845 ) ) ;
#2740 = CARTESIAN_POINT ( 'NONE',  ( 0.000000000000000000, -60.00000000000000000, 0.000000000000000000 ) ) ;
#2741 = CARTESIAN_POINT ( 'NONE',  ( 2.547727811071581527, -7.059815111224851947, -4.314169979798982091 ) ) ;
#2742 = DIRECTION ( 'NONE',  ( -0.000000000000000000, -0.000000000000000000, -1.000000000000000000 ) ) ;
#2743 = CARTESIAN_POINT ( 'NONE',  ( -2.250215587473127332, -47.20000000000001705, 8.376503107917878665 ) ) ;
#2744 = CARTESIAN_POINT ( 'NONE',  ( 0.2999999999999999889, -114.9999999999982236, 0.9539392014169838507 ) ) ;
#2745 = CYLINDRICAL_SURFACE ( 'NONE', #1037, 1.500000000000000444 ) ;
#2746 = CARTESIAN_POINT ( 'NONE',  ( -8.599999999999996092, -50.00000000000000000, -1.366666666666159768 ) ) ;
#2747 = CARTESIAN_POINT ( 'NONE',  ( 11.39539595717845799, -52.79999999999999716, 0.3739757293042010877 ) ) ;
#2748 = CARTESIAN_POINT ( 'NONE',  ( 5.000012828558699773, -48.49995723813396609, 0.09784062508662537405 ) ) ;
#2749 = EDGE_CURVE ( 'NONE', #1883, #439, #2383, .T. ) ;
#2750 = CARTESIAN_POINT ( 'NONE',  ( -8.502540660504315895, -50.22987518539498808, 1.385387373903827157 ) ) ;
#2751 = CARTESIAN_POINT ( 'NONE',  ( -8.599999999999996092, -52.79999999999999716, -1.093333333333363022 ) ) ;
#2752 = AXIS2_PLACEMENT_3D ( 'NONE', #2289, #676, #3202 ) ;
#2753 = VERTEX_POINT ( 'NONE', #967 ) ;
#2754 = CARTESIAN_POINT ( 'NONE',  ( -8.596526774713707297, -50.00000000000000000, 0.2821220414048196679 ) ) ;
#2755 = DIRECTION ( 'NONE',  ( 1.000000000000000000, 0.000000000000000000, 0.000000000000000000 ) ) ;
#2756 = PLANE ( 'NONE',  #2175 ) ;
#2757 = CARTESIAN_POINT ( 'NONE',  ( 0.000000000000000000, 0.000000000000000000, 10.00000000000000000 ) ) ;
#2758 = DIRECTION ( 'NONE',  ( 0.000000000000000000, -0.000000000000000000, -1.000000000000000000 ) ) ;
#2759 = CARTESIAN_POINT ( 'NONE',  ( 0.2999999999999837796, -118.9999999999982379, -0.7416198487096254954 ) ) ;
#2760 = CARTESIAN_POINT ( 'NONE',  ( 11.36325033731732503, -50.00000000000000000, 0.9334869871343942638 ) ) ;
#2761 = CARTESIAN_POINT ( 'NONE',  ( 4.871328134482659777, -49.00786077710490218, -1.129209473734892777 ) ) ;
#2762 = EDGE_CURVE ( 'NONE', #1895, #2919, #981, .T. ) ;
#2763 = CARTESIAN_POINT ( 'NONE',  ( 11.36325033731725576, -52.79999999999999716, 0.9334869871343942638 ) ) ;
#2764 = ORIENTED_EDGE ( 'NONE', *, *, #401, .T. ) ;
#2765 = CARTESIAN_POINT ( 'NONE',  ( 2.543753134549881167, 7.057059595574596500, -4.307653715470421751 ) ) ;
#2766 = PRODUCT_CONTEXT ( 'NONE', #1465, 'mechanical' ) ;
#2767 = DIRECTION ( 'NONE',  ( 0.000000000000000000, 0.000000000000000000, 1.000000000000000000 ) ) ;
#2768 = LINE ( 'NONE', #2281, #1215 ) ;
#2769 = CARTESIAN_POINT ( 'NONE',  ( 0.000000000000000000, 0.000000000000000000, -10.00000000000000000 ) ) ;
#2770 = DIRECTION ( 'NONE',  ( 0.000000000000000000, 0.000000000000000000, -1.000000000000000000 ) ) ;
#2771 = DIRECTION ( 'NONE',  ( 0.000000000000000000, 0.000000000000000000, 1.000000000000000000 ) ) ;
#2772 = CARTESIAN_POINT ( 'NONE',  ( 0.000000000000000000, -80.00000000000000000, 0.000000000000000000 ) ) ;
#2773 = CARTESIAN_POINT ( 'NONE',  ( -8.599999999999996092, -52.79999999999999716, -0.5466666666666361030 ) ) ;
#2774 = ORIENTED_EDGE ( 'NONE', *, *, #291, .F. ) ;
#2775 = CARTESIAN_POINT ( 'NONE',  ( -0.2999999999999999334, -119.0797001093845893, 0.7373211444866922815 ) ) ;
#2776 = ORIENTED_EDGE ( 'NONE', *, *, #1759, .F. ) ;
#2777 = CARTESIAN_POINT ( 'NONE',  ( 1.338285735402328314, 7.387167716089622083, -4.829375120343072147 ) ) ;
#2778 = B_SPLINE_CURVE_WITH_KNOTS ( 'NONE', 3,
 ( #1783, #2533, #2231, #1167, #1523, #2984, #2970, #441, #3237, #185, #262, #964, #1462, #17, #2183, #1981 ),
 .UNSPECIFIED., .F., .F.,
 ( 4, 2, 2, 2, 2, 2, 2, 4 ),
 ( 0.000000000000000000, 0.0004971715929930333941, 0.0009943431859860667882, 0.001988686371972171740, 0.002485857964965238528, 0.002983029557958305749, 0.003480201150951372103, 0.003977372743944438890 ),
 .UNSPECIFIED. ) ;
#2779 = CARTESIAN_POINT ( 'NONE',  ( 1.658007454526697177, -7.321065759480116952, 4.728400501374060205 ) ) ;
#2780 = AXIS2_PLACEMENT_3D ( 'NONE', #57, #2802, #1776 ) ;
#2781 = EDGE_CURVE ( 'NONE', #2412, #1810, #3121, .T. ) ;
#2782 = CARTESIAN_POINT ( 'NONE',  ( -3.117741096646114318, -75.13505426231607487, 3.921983519476101243 ) ) ;
#2783 = EDGE_CURVE ( 'NONE', #3219, #3014, #1487, .T. ) ;
#2784 = DIRECTION ( 'NONE',  ( -0.000000000000000000, -0.000000000000000000, -1.000000000000000000 ) ) ;
#2785 = CARTESIAN_POINT ( 'NONE',  ( -2.300000000000000266, -67.40000000000000568, -1.734723475976807094E-15 ) ) ;
#2786 = LINE ( 'NONE', #1539, #1252 ) ;
#2787 = CARTESIAN_POINT ( 'NONE',  ( 8.160064090060387798, -52.79999999999999716, 2.773119917860402239 ) ) ;
#2788 = ORIENTED_EDGE ( 'NONE', *, *, #2448, .F. ) ;
#2789 = CARTESIAN_POINT ( 'NONE',  ( 6.123233995736765296E-16, -80.00000000000000000, -4.999999999999999112 ) ) ;
#2790 = FILL_AREA_STYLE ('',( #848 ) ) ;
#2791 = AXIS2_PLACEMENT_3D ( 'NONE', #619, #1866, #2088 ) ;
#2792 = DIRECTION ( 'NONE',  ( 0.000000000000000000, 1.000000000000000000, 0.000000000000000000 ) ) ;
#2793 = CARTESIAN_POINT ( 'NONE',  ( 8.485280282859413603, -50.00000000000000000, 1.400000000000001021 ) ) ;
#2794 = VERTEX_POINT ( 'NONE', #2248 ) ;
#2795 = AXIS2_PLACEMENT_3D ( 'NONE', #696, #3003, #725 ) ;
#2796 = CARTESIAN_POINT ( 'NONE',  ( 4.769696007084725409, -50.00000000000000000, -1.500000000000006439 ) ) ;
#2797 = CARTESIAN_POINT ( 'NONE',  ( 8.600005876649037262, -47.20000000000001705, -0.2541998246239300374 ) ) ;
#2798 = STYLED_ITEM ( 'NONE', ( #2337 ), #2473 ) ;
#2799 = SHAPE_REPRESENTATION ( 'thread guide', ( #1692 ), #1379 ) ;
#2800 = CARTESIAN_POINT ( 'NONE',  ( -1.696011499264676647, -75.76451282912192653, 4.715485471644024429 ) ) ;
#2801 = DIRECTION ( 'NONE',  ( 1.000000000000000000, 0.000000000000000000, 0.000000000000000000 ) ) ;
#2802 = DIRECTION ( 'NONE',  ( -0.000000000000000000, -0.000000000000000000, -1.000000000000000000 ) ) ;
#2803 = PLANE ( 'NONE',  #3163 ) ;
#2804 = CARTESIAN_POINT ( 'NONE',  ( -8.324422814933019055, -50.00000000000000000, 2.231815450536601464 ) ) ;
#2805 = EDGE_LOOP ( 'NONE', ( #2058, #2565 ) ) ;
#2806 = CARTESIAN_POINT ( 'NONE',  ( 0.3000000000000000444, -114.9201045547228119, -0.9581268606072532723 ) ) ;
#2807 = SURFACE_SIDE_STYLE ('',( #2861 ) ) ;
#2808 = CARTESIAN_POINT ( 'NONE',  ( 7.513445500750180805, -50.00000000000000000, 4.333070140107198043 ) ) ;
#2809 = CARTESIAN_POINT ( 'NONE',  ( 8.160064090060387798, -50.00000000000000000, 2.773119917860402239 ) ) ;
#2810 = ORIENTED_EDGE ( 'NONE', *, *, #1084, .T. ) ;
#2811 = CARTESIAN_POINT ( 'NONE',  ( 2.816687638038912549E-16, -84.99999999999998579, -2.300000000000000266 ) ) ;
#2812 = CARTESIAN_POINT ( 'NONE',  ( -8.530791689320901483, -47.20000000000001705, 1.124695299888049504 ) ) ;
#2813 = ORIENTED_EDGE ( 'NONE', *, *, #433, .F. ) ;
#2814 = CARTESIAN_POINT ( 'NONE',  ( -4.985642101603771081, -51.45153962441924733, 0.3907762206522687465 ) ) ;
#2815 = LINE ( 'NONE', #2298, #729 ) ;
#2816 = EDGE_LOOP ( 'NONE', ( #612, #2820, #795, #70 ) ) ;
#2817 =( NAMED_UNIT ( * ) SI_UNIT ( $, .STERADIAN. ) SOLID_ANGLE_UNIT ( ) );
#2818 = DIRECTION ( 'NONE',  ( 0.000000000000000000, 0.000000000000000000, 1.000000000000000000 ) ) ;
#2819 = CARTESIAN_POINT ( 'NONE',  ( -4.331939449206426929, -52.79999999999999716, 7.514224851276242845 ) ) ;
#2820 = ORIENTED_EDGE ( 'NONE', *, *, #983, .F. ) ;
#2821 = CARTESIAN_POINT ( 'NONE',  ( 2.348910296171192290E-13, -114.6999999999962228, -1.015000000000727765 ) ) ;
#2822 = EDGE_CURVE ( 'NONE', #1087, #3085, #1793, .T. ) ;
#2823 = CARTESIAN_POINT ( 'NONE',  ( -1.125736483476999839, -50.00000000000000000, 8.599999999999996092 ) ) ;
#2824 = CARTESIAN_POINT ( 'NONE',  ( 8.485280282859413603, -50.00000000000000000, 1.400000000000001021 ) ) ;
#2825 = VERTEX_POINT ( 'NONE', #204 ) ;
#2826 = CARTESIAN_POINT ( 'NONE',  ( 4.828226831489238258, -50.75376282162932995, 1.300528505912509125 ) ) ;
#2827 = VECTOR ( 'NONE', #852, 1000.000000000000000 ) ;
#2828 = B_SPLINE_CURVE_WITH_KNOTS ( 'NONE', 3,
 ( #3060, #2775, #1557, #298, #2072, #518 ),
 .UNSPECIFIED., .F., .F.,
 ( 4, 2, 4 ),
 ( 1.973474095025335319E-07, 0.0002361394426573917090, 0.0004720815379052808731 ),
 .UNSPECIFIED. ) ;
#2829 = CARTESIAN_POINT ( 'NONE',  ( -11.39999532361432522, -47.20000000000001705, 0.1755699507458657049 ) ) ;
#2830 = AXIS2_PLACEMENT_3D ( 'NONE', #1055, #1815, #2008 ) ;
#2831 = CARTESIAN_POINT ( 'NONE',  ( -4.828108292616975383, -50.75302333124540866, -1.300971953686710592 ) ) ;
#2832 = VECTOR ( 'NONE', #1552, 1000.000000000000000 ) ;
#2833 = CARTESIAN_POINT ( 'NONE',  ( 0.000000000000000000, -118.9999999999982379, -2.300000000000000266 ) ) ;
#2834 = ORIENTED_EDGE ( 'NONE', *, *, #230, .F. ) ;
#2835 = FILL_AREA_STYLE_COLOUR ( '', #2909 ) ;
#2836 = CARTESIAN_POINT ( 'NONE',  ( 3.061616997868383634E-16, -60.00000000000000000, 2.500000000000000444 ) ) ;
#2837 = CARTESIAN_POINT ( 'NONE',  ( 8.582665138674004268, -52.79999999999999716, 0.5636706063485154017 ) ) ;
#2838 = ORIENTED_EDGE ( 'NONE', *, *, #3240, .F. ) ;
#2839 = CARTESIAN_POINT ( 'NONE',  ( 0.000000000000000000, 80.00000000000000000, 0.000000000000000000 ) ) ;
#2840 = EDGE_CURVE ( 'NONE', #342, #3085, #1449, .T. ) ;
#2841 = CARTESIAN_POINT ( 'NONE',  ( 0.000000000000000000, -67.50000000000000000, -2.500000000000000444 ) ) ;
#2842 = CYLINDRICAL_SURFACE ( 'NONE', #259, 1.499999999999999778 ) ;
#2843 = LINE ( 'NONE', #1785, #630 ) ;
#2844 = ORIENTED_EDGE ( 'NONE', *, *, #15, .F. ) ;
#2845 = CARTESIAN_POINT ( 'NONE',  ( -4.666223265025314149, 5.872199985543652190, 1.803446265377422364 ) ) ;
#2846 = CIRCLE ( 'NONE', #529, 1.499999999999999778 ) ;
#2847 = CARTESIAN_POINT ( 'NONE',  ( -9.116201041289377471, -47.20000000000001705, 7.005833569791151128 ) ) ;
#2848 = EDGE_CURVE ( 'NONE', #1926, #1054, #492, .T. ) ;
#2849 = AXIS2_PLACEMENT_3D ( 'NONE', #709, #1997, #2934 ) ;
#2850 = DIRECTION ( 'NONE',  ( -1.000000000000000000, -0.000000000000000000, -0.000000000000000000 ) ) ;
#2851 = PRESENTATION_LAYER_ASSIGNMENT (  '', '', ( #2437 ) ) ;
#2852 = EDGE_CURVE ( 'NONE', #1036, #1926, #3175, .T. ) ;
#2853 = CARTESIAN_POINT ( 'NONE',  ( -7.513445500749800665, -50.00000000000000000, 4.333070140105378165 ) ) ;
#2854 = ORIENTED_EDGE ( 'NONE', *, *, #553, .F. ) ;
#2855 = ADVANCED_FACE ( 'NONE', ( #2428 ), #153, .F. ) ;
#2856 = SURFACE_STYLE_USAGE ( .BOTH. , #1152 ) ;
#2857 = CARTESIAN_POINT ( 'NONE',  ( -5.000000000000000000, 30.00000000000000000, -21.62277660168378901 ) ) ;
#2858 = CARTESIAN_POINT ( 'NONE',  ( 8.530791689320606608, -52.79999999999999716, 1.124695299888175182 ) ) ;
#2859 = ORIENTED_EDGE ( 'NONE', *, *, #1414, .F. ) ;
#2860 = FACE_OUTER_BOUND ( 'NONE', #1497, .T. ) ;
#2861 = SURFACE_STYLE_FILL_AREA ( #2790 ) ;
#2862 = CARTESIAN_POINT ( 'NONE',  ( 3.971589419094359030, 6.365665093354385462, -3.054047635831909524 ) ) ;
#2863 = CARTESIAN_POINT ( 'NONE',  ( -0.8700260635408603171, -64.06095412063420724, 4.926729975457289967 ) ) ;
#2864 = ORIENTED_EDGE ( 'NONE', *, *, #2004, .T. ) ;
#2865 = CARTESIAN_POINT ( 'NONE',  ( -2.300000000000000266, -67.40000000000000568, -1.734723475976807094E-15 ) ) ;
#2866 = CARTESIAN_POINT ( 'NONE',  ( 9.959683570760574867, -50.00000000000000000, 5.743837162466680191 ) ) ;
#2867 = CARTESIAN_POINT ( 'NONE',  ( -8.555056788725856620, -49.54949886534770087, 1.341113681525112122 ) ) ;
#2868 = EDGE_CURVE ( 'NONE', #1046, #2883, #3228, .T. ) ;
#2869 = CARTESIAN_POINT ( 'NONE',  ( -8.469856736028225086, -50.00000000000000000, 1.493482969799723170 ) ) ;
#2870 = VERTEX_POINT ( 'NONE', #3239 ) ;
#2871 = CARTESIAN_POINT ( 'NONE',  ( -1.984638188030386718, -68.47121416379373215, -4.590313865678165683 ) ) ;
#2872 = LINE ( 'NONE', #1619, #93 ) ;
#2873 = B_SPLINE_CURVE_WITH_KNOTS ( 'NONE', 3,
 ( #2965, #2490, #2735, #1443, #2193, #149, #1226, #2945, #3212, #926, #1737, #452, #212, #1940 ),
 .UNSPECIFIED., .F., .F.,
 ( 4, 2, 2, 2, 2, 2, 4 ),
 ( -7.483321455836769026E-06, 0.0006606241027954191589, 0.001328731527046675062, 0.001662785239172306700, 0.001996838951297938338, 0.002330892663423569759, 0.002664946375549201180 ),
 .UNSPECIFIED. ) ;
#2874 = PLANE ( 'NONE',  #47 ) ;
#2875 = ORIENTED_EDGE ( 'NONE', *, *, #2906, .T. ) ;
#2876 = DIRECTION ( 'NONE',  ( -1.000000000000000000, 0.000000000000000000, 0.000000000000000000 ) ) ;
#2877 = CARTESIAN_POINT ( 'NONE',  ( 2.258341722794894313, 7.158742388247099520, 4.472964013438597952 ) ) ;
#2878 = CARTESIAN_POINT ( 'NONE',  ( -11.39999999999999680, -47.20000000000001705, -1.366666666666159546 ) ) ;
#2879 = CARTESIAN_POINT ( 'NONE',  ( -2.681043805932831425, -7.005876582393428365, -4.223450101800680478 ) ) ;
#2880 = EDGE_LOOP ( 'NONE', ( #2552, #1949, #1637, #2475 ) ) ;
#2881 = CARTESIAN_POINT ( 'NONE',  ( 8.572527594031472993E-15, -70.00000000000000000, 10.00000000000000000 ) ) ;
#2882 = CARTESIAN_POINT ( 'NONE',  ( -11.39999999999999680, -52.79999999999999716, -0.5466666666666361030 ) ) ;
#2883 = VERTEX_POINT ( 'NONE', #2497 ) ;
#2884 = DIRECTION ( 'NONE',  ( 0.000000000000000000, 0.000000000000000000, -1.000000000000000000 ) ) ;
#2885 = AXIS2_PLACEMENT_3D ( 'NONE', #142, #2699, #905 ) ;
#2886 = ADVANCED_FACE ( 'NONE', ( #220 ), #1232, .F. ) ;
#2887 = ORIENTED_EDGE ( 'NONE', *, *, #1442, .F. ) ;
#2888 = FACE_OUTER_BOUND ( 'NONE', #913, .T. ) ;
#2889 = CARTESIAN_POINT ( 'NONE',  ( 0.000000000000000000, 0.000000000000000000, 10.00000000000000000 ) ) ;
#2890 = CARTESIAN_POINT ( 'NONE',  ( 2.416866957515810821, -69.33968019788672166, -4.377234380186135532 ) ) ;
#2891 = ORIENTED_EDGE ( 'NONE', *, *, #889, .T. ) ;
#2892 = ADVANCED_FACE ( 'NONE', ( #1746 ), #2756, .T. ) ;
#2893 = CIRCLE ( 'NONE', #404, 2.500000000000000444 ) ;
#2894 =( NAMED_UNIT ( * ) PLANE_ANGLE_UNIT ( ) SI_UNIT ( $, .RADIAN. ) );
#2895 = CARTESIAN_POINT ( 'NONE',  ( -11.39999532361432522, -50.00000000000000000, 0.1755699507458657049 ) ) ;
#2896 = CARTESIAN_POINT ( 'NONE',  ( 2.500000000000003553, -68.53553390593273775, 1.464466094067263358 ) ) ;
#2897 = CARTESIAN_POINT ( 'NONE',  ( -4.865239396163736352, 5.708012565174444219, -1.165122949380803741 ) ) ;
#2898 = CARTESIAN_POINT ( 'NONE',  ( 11.36325033731739609, -47.20000000000001705, 0.9334869871343942638 ) ) ;
#2899 = ORIENTED_EDGE ( 'NONE', *, *, #2954, .F. ) ;
#2900 = B_SPLINE_CURVE_WITH_KNOTS ( 'NONE', 3,
 ( #1530, #7, #55, #2044, #1791, #769, #2800, #2080, #1015, #2782, #1295, #2311, #39, #1047, #2060, #803, #1562, #2571, #305, #1314, #3123, #2113, #1149, #1365 ),
 .UNSPECIFIED., .F., .F.,
 ( 4, 2, 2, 2, 2, 2, 2, 2, 2, 2, 2, 4 ),
 ( 0.008369288751650577618, 0.008891570837864931631, 0.009413852924079285645, 0.01045841709650799888, 0.01150298126893671384, 0.01254754544136542707, 0.01359210961379414204, 0.01463667378622285700, 0.01515895587243721448, 0.01568123795865156850, 0.01620352004486592945, 0.01672580213108028693 ),
 .UNSPECIFIED. ) ;
#2901 = CARTESIAN_POINT ( 'NONE',  ( 0.000000000000000000, -84.99999999999998579, 2.300000000000000266 ) ) ;
#2902 = VECTOR ( 'NONE', #1903, 1000.000000000000000 ) ;
#2903 = EDGE_LOOP ( 'NONE', ( #2854, #637 ) ) ;
#2904 = CIRCLE ( 'NONE', #1162, 7.500000000000000000 ) ;
#2905 =( LENGTH_UNIT ( ) NAMED_UNIT ( * ) SI_UNIT ( .MILLI., .METRE. ) );
#2906 = EDGE_CURVE ( 'NONE', #2611, #1146, #2079, .T. ) ;
#2907 = CARTESIAN_POINT ( 'NONE',  ( -8.599999999999996092, -50.00000000000000000, -1.639999999999997460 ) ) ;
#2908 = CARTESIAN_POINT ( 'NONE',  ( 9.198767304811504175, -48.81800434884510764, 0.7702149575309279461 ) ) ;
#2909 = COLOUR_RGB ( '',0.8941176470588234615, 0.8941176470588234615, 0.8941176470588234615 ) ;
#2910 = ORIENTED_EDGE ( 'NONE', *, *, #1553, .F. ) ;
#2911 = CARTESIAN_POINT ( 'NONE',  ( -7.500000000000000000, 0.000000000000000000, 10.00000000000000000 ) ) ;
#2912 = EDGE_CURVE ( 'NONE', #3219, #1139, #1000, .T. ) ;
#2913 = CARTESIAN_POINT ( 'NONE',  ( 1.492255338562904265, -47.20000000000001705, 11.39999999999999680 ) ) ;
#2914 = CARTESIAN_POINT ( 'NONE',  ( -11.03470001049207916, -50.00000000000000000, 2.958453039083848601 ) ) ;
#2915 = PLANE ( 'NONE',  #1088 ) ;
#2916 = CARTESIAN_POINT ( 'NONE',  ( -11.39999532361432522, -50.00000000000000000, 0.1755699507458657049 ) ) ;
#2917 = ORIENTED_EDGE ( 'NONE', *, *, #1884, .F. ) ;
#2918 = CARTESIAN_POINT ( 'NONE',  ( -2.417990129674731481, -70.65652927704230990, -4.376613296505728279 ) ) ;
#2919 = VERTEX_POINT ( 'NONE', #2295 ) ;
#2920 = CARTESIAN_POINT ( 'NONE',  ( -2.499999999999991118, -70.00000000000000000, -4.330127018922196314 ) ) ;
#2921 = CARTESIAN_POINT ( 'NONE',  ( 8.572527594031472993E-15, -70.00000000000000000, 10.00000000000000000 ) ) ;
#2922 = CARTESIAN_POINT ( 'NONE',  ( 2.482721767081392361, -69.66330910517966402, -4.340221116104048704 ) ) ;
#2923 = VERTEX_POINT ( 'NONE', #3068 ) ;
#2924 = CARTESIAN_POINT ( 'NONE',  ( -4.916186798144710934, -48.80118439239116412, 0.9225820817148873143 ) ) ;
#2925 =( BOUNDED_CURVE ( )  B_SPLINE_CURVE ( 3, ( #64, #3094, #1833, #2841 ),
 .UNSPECIFIED., .F., .F. ) 
 B_SPLINE_CURVE_WITH_KNOTS ( ( 4, 4 ),
 ( 1.570796326794896558, 3.141592653589791340 ),
 .UNSPECIFIED. ) 
 CURVE ( )  GEOMETRIC_REPRESENTATION_ITEM ( )  RATIONAL_B_SPLINE_CURVE ( ( 1.000000000000000000, 0.8047378541243654926, 0.8047378541243654926, 1.000000000000000000 ) ) 
 REPRESENTATION_ITEM ( '' )  );
#2926 = CARTESIAN_POINT ( 'NONE',  ( -11.03470001049207916, -50.00000000000000000, 2.958453039083848601 ) ) ;
#2927 = FILL_AREA_STYLE_COLOUR ( '', #1409 ) ;
#2928 = ADVANCED_FACE ( 'NONE', ( #1030 ), #2555, .F. ) ;
#2929 = CARTESIAN_POINT ( 'NONE',  ( 0.2669266955305334976, -119.1574544647984766, -0.7479247211079949054 ) ) ;
#2930 = CARTESIAN_POINT ( 'NONE',  ( 11.39999999999999680, -47.20000000000001705, -1.093333333333372126 ) ) ;
#2931 = EDGE_LOOP ( 'NONE', ( #2480, #2446, #2723, #2917 ) ) ;
#2932 = CARTESIAN_POINT ( 'NONE',  ( 8.530791689320606608, -47.20000000000001705, 1.124695299888175182 ) ) ;
#2933 = FACE_OUTER_BOUND ( 'NONE', #2931, .T. ) ;
#2934 = DIRECTION ( 'NONE',  ( 0.000000000000000000, 0.000000000000000000, -1.000000000000000000 ) ) ;
#2935 = ORIENTED_EDGE ( 'NONE', *, *, #966, .T. ) ;
#2936 = CARTESIAN_POINT ( 'NONE',  ( 0.000000000000000000, 30.00000000000000000, 10.00000000000000000 ) ) ;
#2937 = VECTOR ( 'NONE', #46, 1000.000000000000000 ) ;
#2938 = CARTESIAN_POINT ( 'NONE',  ( -8.324422814933019055, -50.00000000000000000, 2.231815450536601464 ) ) ;
#2939 = CARTESIAN_POINT ( 'NONE',  ( 8.555056788725931227, -49.54949886534768666, 1.341113681525113455 ) ) ;
#2940 = CARTESIAN_POINT ( 'NONE',  ( 2.312079649032892981, -75.54619300223156131, 4.445949067509105568 ) ) ;
#2941 = CARTESIAN_POINT ( 'NONE',  ( -4.916102558146631551, -48.80163753725855003, -0.9228986618089604077 ) ) ;
#2942 = AXIS2_PLACEMENT_3D ( 'NONE', #2833, #2513, #1763 ) ;
#2943 = CARTESIAN_POINT ( 'NONE',  ( 8.599999999999996092, -47.20000000000001705, -1.639999999999997460 ) ) ;
#2944 = CARTESIAN_POINT ( 'NONE',  ( -5.742338339643776379, -50.00000000000000000, 9.960716663318299524 ) ) ;
#2945 = CARTESIAN_POINT ( 'NONE',  ( -11.15228598338264909, -50.80068377669682178, -1.152285983382659751 ) ) ;
#2946 = VECTOR ( 'NONE', #2119, 1000.000000000000000 ) ;
#2947 = EDGE_CURVE ( 'NONE', #1384, #3070, #2768, .T. ) ;
#2948 =( BOUNDED_CURVE ( )  B_SPLINE_CURVE ( 3, ( #1885, #2141, #2123, #602 ),
 .UNSPECIFIED., .F., .T. ) 
 B_SPLINE_CURVE_WITH_KNOTS ( ( 4, 4 ),
 ( 0.000000000000000000, 1.570796326794896780 ),
 .UNSPECIFIED. ) 
 CURVE ( )  GEOMETRIC_REPRESENTATION_ITEM ( )  RATIONAL_B_SPLINE_CURVE ( ( 1.000000000000000000, 0.8047378541243649375, 0.8047378541243649375, 1.000000000000000000 ) ) 
 REPRESENTATION_ITEM ( '' )  );
#2949 = CARTESIAN_POINT ( 'NONE',  ( 8.160064090060387798, -52.79999999999999716, 2.773119917860402239 ) ) ;
#2950 = ORIENTED_EDGE ( 'NONE', *, *, #3253, .F. ) ;
#2951 = CARTESIAN_POINT ( 'NONE',  ( 8.599999999999996092, -50.00000000000000000, -1.093333333333372126 ) ) ;
#2952 = CARTESIAN_POINT ( 'NONE',  ( 6.123233995736538006E-17, -125.0000000000000000, -0.4999999999999813483 ) ) ;
#2953 = DIRECTION ( 'NONE',  ( -0.000000000000000000, -1.000000000000000000, -0.000000000000000000 ) ) ;
#2954 = EDGE_CURVE ( 'NONE', #129, #3266, #2900, .T. ) ;
#2955 = ORIENTED_EDGE ( 'NONE', *, *, #1230, .T. ) ;
#2956 = DIRECTION ( 'NONE',  ( 0.000000000000000000, 0.000000000000000000, 1.000000000000000000 ) ) ;
#2957 = VECTOR ( 'NONE', #1638, 1000.000000000000000 ) ;
#2958 = CARTESIAN_POINT ( 'NONE',  ( -8.160064090060583197, -50.00000000000000000, 2.773119917861301964 ) ) ;
#2959 = CARTESIAN_POINT ( 'NONE',  ( 2.500000000000003109, -68.53553390593273775, -1.464466094067265134 ) ) ;
#2960 = CARTESIAN_POINT ( 'NONE',  ( 0.000000000000000000, 0.000000000000000000, 18.00000000000000355 ) ) ;
#2961 = AXIS2_PLACEMENT_3D ( 'NONE', #2985, #3217, #677 ) ;
#2962 = PLANE ( 'NONE',  #3171 ) ;
#2963 = CARTESIAN_POINT ( 'NONE',  ( -11.25335008359243005, -52.79999999999999716, 1.860476840075229843 ) ) ;
#2964 = CARTESIAN_POINT ( 'NONE',  ( 4.997016223860688555, -48.50986200051738706, 0.1978941090189494934 ) ) ;
#2965 = CARTESIAN_POINT ( 'NONE',  ( -10.00000000000001776, -51.39999999999999858, 1.734719586992576771E-19 ) ) ;
#2966 = B_SPLINE_CURVE_WITH_KNOTS ( 'NONE', 3,
 ( #2362, #2869, #1081, #1332, #2097, #2853, #1599, #341, #1348, #91, #1100, #3124, #1366, #2537, #1324, #3096, #83, #2809, #1092, #1340, #1818, #2793 ),
 .UNSPECIFIED., .F., .F.,
 ( 4, 2, 2, 2, 2, 2, 2, 2, 2, 2, 4 ),
 ( 0.05198376726129744912, 0.06250000000000000000, 0.1250000000000000000, 0.2500000000000000000, 0.3750000000000000000, 0.5000000000000000000, 0.6250000000000000000, 0.7500000000000000000, 0.8750000000000000000, 0.9375000000000000000, 0.9480162327386928434 ),
 .UNSPECIFIED. ) ;
#2967 = CARTESIAN_POINT ( 'NONE',  ( 7.513445500750181694, -52.79999999999999716, 4.333070140107198043 ) ) ;
#2968 = ORIENTED_EDGE ( 'NONE', *, *, #507, .T. ) ;
#2969 = CARTESIAN_POINT ( 'NONE',  ( -8.599999999999996092, -47.20000000000001705, -0.5466666666666361030 ) ) ;
#2970 = CARTESIAN_POINT ( 'NONE',  ( 1.994666228034125410, -71.54083103000799326, -4.591303954161849887 ) ) ;
#2971 = FACE_OUTER_BOUND ( 'NONE', #2626, .T. ) ;
#2972 = ORIENTED_EDGE ( 'NONE', *, *, #1919, .F. ) ;
#2973 = DIRECTION ( 'NONE',  ( -0.000000000000000000, -0.000000000000000000, 1.000000000000000000 ) ) ;
#2974 = CARTESIAN_POINT ( 'NONE',  ( -8.596526774713707297, -50.00000000000000000, 0.2821220414048196679 ) ) ;
#2975 = FACE_BOUND ( 'NONE', #2136, .T. ) ;
#2976 = DIRECTION ( 'NONE',  ( 0.000000000000000000, 0.000000000000000000, 1.000000000000000000 ) ) ;
#2977 = CARTESIAN_POINT ( 'NONE',  ( 0.000000000000000000, 0.000000000000000000, 18.00000000000000355 ) ) ;
#2978 = CARTESIAN_POINT ( 'NONE',  ( -11.39999999999999680, -52.79999999999999716, -1.366666666666159546 ) ) ;
#2979 = CARTESIAN_POINT ( 'NONE',  ( 9.116201041287551377, -50.00000000000000000, 7.005833569791843018 ) ) ;
#2980 = CARTESIAN_POINT ( 'NONE',  ( 0.2999999999999837796, -118.9999999999982379, -0.7416198487096254954 ) ) ;
#2981 = CARTESIAN_POINT ( 'NONE',  ( 8.599999999999996092, -52.79999999999999716, -1.093333333333372126 ) ) ;
#2982 = ORIENTED_EDGE ( 'NONE', *, *, #811, .F. ) ;
#2983 = CARTESIAN_POINT ( 'NONE',  ( 8.599996472200352571, -50.00000000000000000, 0.1525981975067866592 ) ) ;
#2984 = CARTESIAN_POINT ( 'NONE',  ( 2.179086395304381085, -71.26814162161134902, -4.502426019400062707 ) ) ;
#2985 = CARTESIAN_POINT ( 'NONE',  ( -2.300000000000000266, -67.40000000000000568, -1.734723475976807094E-15 ) ) ;
#2986 = APPLICATION_CONTEXT ( 'automotive_design' ) ;
#2987 = DIRECTION ( 'NONE',  ( 0.000000000000000000, 0.000000000000000000, 1.000000000000000000 ) ) ;
#2988 = EDGE_CURVE ( 'NONE', #2883, #1087, #1639, .T. ) ;
#2989 = CARTESIAN_POINT ( 'NONE',  ( -5.742338339643776379, -47.20000000000001705, 9.960716663318299524 ) ) ;
#2990 = CARTESIAN_POINT ( 'NONE',  ( 0.000000000000000000, 30.00000000000000000, 18.00000000000000355 ) ) ;
#2991 = CARTESIAN_POINT ( 'NONE',  ( 3.791988745706118547, -74.65761308588932366, 3.273615902745502737 ) ) ;
#2992 = CARTESIAN_POINT ( 'NONE',  ( -8.599999999999996092, -50.00000000000000000, -1.093333333333363022 ) ) ;
#2993 = CARTESIAN_POINT ( 'NONE',  ( -11.39999999999999680, -52.79999999999999716, -1.639999999999997460 ) ) ;
#2994 = CARTESIAN_POINT ( 'NONE',  ( 11.30825875096028099, -50.00000000000000000, 1.490875164968454181 ) ) ;
#2995 = VECTOR ( 'NONE', #2540, 1000.000000000000000 ) ;
#2996 = CARTESIAN_POINT ( 'NONE',  ( -8.564669657330886920, -50.44377267524131270, 1.332368788789987768 ) ) ;
#2997 = CIRCLE ( 'NONE', #2684, 4.999999999999999112 ) ;
#2998 = CARTESIAN_POINT ( 'NONE',  ( -8.599999999999996092, -50.00000000000000000, -1.093333333333363022 ) ) ;
#2999 = EDGE_CURVE ( 'NONE', #102, #1865, #2613, .T. ) ;
#3000 = VERTEX_POINT ( 'NONE', #1857 ) ;
#3001 = CARTESIAN_POINT ( 'NONE',  ( 6.877134118866901957, -47.20000000000001705, 5.285102517562147995 ) ) ;
#3002 = CARTESIAN_POINT ( 'NONE',  ( 10.31385090661579795, -48.62614420630679746, -0.3138474430211479760 ) ) ;
#3003 = DIRECTION ( 'NONE',  ( 0.000000000000000000, 0.000000000000000000, 1.000000000000000000 ) ) ;
#3004 = CARTESIAN_POINT ( 'NONE',  ( -6.877134118866001344, -47.20000000000001705, 5.285102517561345969 ) ) ;
#3005 = CARTESIAN_POINT ( 'NONE',  ( -10.76729745289139473, -48.81576204415910070, -0.7672974528914079384 ) ) ;
#3006 = DIRECTION ( 'NONE',  ( 1.000000000000000000, 0.000000000000000000, 0.000000000000000000 ) ) ;
#3007 = CIRCLE ( 'NONE', #1424, 7.500000000000000000 ) ;
#3008 = CARTESIAN_POINT ( 'NONE',  ( 8.485280282859415379, -50.11569792258605816, 1.400000000000001243 ) ) ;
#3009 = CARTESIAN_POINT ( 'NONE',  ( 11.39999999999999680, -52.79999999999999716, -1.366666666666861873 ) ) ;
#3010 = AXIS2_PLACEMENT_3D ( 'NONE', #3203, #1727, #1199 ) ;
#3011 = CARTESIAN_POINT ( 'NONE',  ( 4.828108292616975383, -49.24697666875461977, -1.300971953686710592 ) ) ;
#3012 =( NAMED_UNIT ( * ) SI_UNIT ( $, .STERADIAN. ) SOLID_ANGLE_UNIT ( ) );
#3013 = CARTESIAN_POINT ( 'NONE',  ( -7.513445500749801553, -52.79999999999999716, 4.333070140105379942 ) ) ;
#3014 = VERTEX_POINT ( 'NONE', #1347 ) ;
#3015 = CARTESIAN_POINT ( 'NONE',  ( 0.000000000000000000, 0.000000000000000000, 10.00000000000000000 ) ) ;
#3016 = SHAPE_DEFINITION_REPRESENTATION ( #886, #1236 ) ;
#3017 = CARTESIAN_POINT ( 'NONE',  ( 3.071765256614000794, -6.848070662608381376, 3.958153484541630629 ) ) ;
#3018 = CARTESIAN_POINT ( 'NONE',  ( -4.999974214802088035, -51.49991404933287953, -0.1976414581757740541 ) ) ;
#3019 = UNCERTAINTY_MEASURE_WITH_UNIT (LENGTH_MEASURE( 1.000000000000000082E-05 ), #2071, 'distance_accuracy_value', 'NONE');
#3020 = DIRECTION ( 'NONE',  ( -1.000000000000000000, -0.000000000000000000, -0.000000000000000000 ) ) ;
#3021 = CARTESIAN_POINT ( 'NONE',  ( -0.1569248533674518220, -119.2672972209964257, -0.7728889768974923635 ) ) ;
#3022 = PLANE ( 'NONE',  #2525 ) ;
#3023 = CARTESIAN_POINT ( 'NONE',  ( 11.39999532361432522, -50.00000000000000000, 0.1755699507458462760 ) ) ;
#3024 = ORIENTED_EDGE ( 'NONE', *, *, #3087, .F. ) ;
#3025 = EDGE_CURVE ( 'NONE', #661, #365, #3055, .T. ) ;
#3026 = CARTESIAN_POINT ( 'NONE',  ( 8.599999999999996092, -50.00000000000000000, -1.366666666666861873 ) ) ;
#3027 = ORIENTED_EDGE ( 'NONE', *, *, #672, .F. ) ;
#3028 = FACE_OUTER_BOUND ( 'NONE', #330, .T. ) ;
#3029 = CARTESIAN_POINT ( 'NONE',  ( -4.823113930341510702, -66.42898515000459270, 1.361197559098670018 ) ) ;
#3030 = CARTESIAN_POINT ( 'NONE',  ( -4.815110478384604598, -50.66583824856825657, 1.347678760471933135 ) ) ;
#3031 = LINE ( 'NONE', #1016, #1902 ) ;
#3032 = CARTESIAN_POINT ( 'NONE',  ( -0.07888090825136341577, -119.2999999999982208, -0.7850000000000491029 ) ) ;
#3033 = DIRECTION ( 'NONE',  ( 0.000000000000000000, 0.000000000000000000, 1.000000000000000000 ) ) ;
#3034 = CARTESIAN_POINT ( 'NONE',  ( 0.2999999999999837796, -117.6667274285785112, -0.8135312234519487262 ) ) ;
#3035 = CARTESIAN_POINT ( 'NONE',  ( -5.285102517542626721, -52.79999999999999716, 6.877134118847253674 ) ) ;
#3036 = VERTEX_POINT ( 'NONE', #873 ) ;
#3037 = LINE ( 'NONE', #2952, #1005 ) ;
#3038 = COLOUR_RGB ( '',0.8941176470588234615, 0.8941176470588234615, 0.8941176470588234615 ) ;
#3039 = CYLINDRICAL_SURFACE ( 'NONE', #2309, 2.499999999999999556 ) ;
#3040 = DIRECTION ( 'NONE',  ( -1.000000000000000000, -0.000000000000000000, -0.000000000000000000 ) ) ;
#3041 = ORIENTED_EDGE ( 'NONE', *, *, #3118, .F. ) ;
#3042 = CARTESIAN_POINT ( 'NONE',  ( 4.815134987083422580, -50.66601675922331083, 1.347591700989805741 ) ) ;
#3043 = EDGE_CURVE ( 'NONE', #1754, #3000, #3104, .T. ) ;
#3044 = ITEM_DEFINED_TRANSFORMATION ( 'NONE', 'NONE', #955,  #1692 ) ;
#3045 =( REPRESENTATION_RELATIONSHIP ('NONE','NONE', #545, #457 ) REPRESENTATION_RELATIONSHIP_WITH_TRANSFORMATION ( #2076 )SHAPE_REPRESENTATION_RELATIONSHIP( ) );
#3046 = AXIS2_PLACEMENT_3D ( 'NONE', #2041, #1802, #1558 ) ;
#3047 = CARTESIAN_POINT ( 'NONE',  ( -4.916145513835878944, -51.19865504686695346, 0.9228047480949569392 ) ) ;
#3048 = UNCERTAINTY_MEASURE_WITH_UNIT (LENGTH_MEASURE( 1.000000000000000082E-05 ), #30, 'distance_accuracy_value', 'NONE');
#3049 = CARTESIAN_POINT ( 'NONE',  ( 6.123233995736538006E-17, -125.0000000000000000, -0.4999999999999813483 ) ) ;
#3050 = CARTESIAN_POINT ( 'NONE',  ( -0.2671776428992062580, -119.1571283586499561, -0.7478606154414338958 ) ) ;
#3051 =( NAMED_UNIT ( * ) PLANE_ANGLE_UNIT ( ) SI_UNIT ( $, .RADIAN. ) );
#3052 = CARTESIAN_POINT ( 'NONE',  ( -7.500000000000000000, -50.00000000000000000, -6.123233995736766085E-15 ) ) ;
#3053 = CARTESIAN_POINT ( 'NONE',  ( 7.513445500750181694, -52.79999999999999716, 4.333070140107198043 ) ) ;
#3054 = ORIENTED_EDGE ( 'NONE', *, *, #547, .F. ) ;
#3055 = B_SPLINE_CURVE_WITH_KNOTS ( 'NONE', 3,
 ( #2379, #1099, #2867, #137, #1660, #2164, #629, #2674, #3172, #660, #610, #1615 ),
 .UNSPECIFIED., .F., .F.,
 ( 4, 2, 2, 2, 2, 4 ),
 ( 0.002704438958044351297, 0.003382491784598461778, 0.004060544611152572259, 0.004738597437706682305, 0.005077623850983738196, 0.005416650264260793220 ),
 .UNSPECIFIED. ) ;
#3056 =( NAMED_UNIT ( * ) SI_UNIT ( $, .STERADIAN. ) SOLID_ANGLE_UNIT ( ) );
#3057 = PRODUCT_DEFINITION ( 'UNKNOWN', '', #856, #1001 ) ;
#3058 =( NAMED_UNIT ( * ) SI_UNIT ( $, .STERADIAN. ) SOLID_ANGLE_UNIT ( ) );
#3059 = VECTOR ( 'NONE', #1514, 1000.000000000000000 ) ;
#3060 = CARTESIAN_POINT ( 'NONE',  ( -0.3000000000000161982, -118.9999999999982379, 0.7416198487096099523 ) ) ;
#3061 = CARTESIAN_POINT ( 'NONE',  ( -4.829496642845706234, -5.738802261244866365, 1.336683695250854953 ) ) ;
#3062 = ORIENTED_EDGE ( 'NONE', *, *, #925, .F. ) ;
#3063 = AXIS2_PLACEMENT_3D ( 'NONE', #3190, #235, #918 ) ;
#3064 = CARTESIAN_POINT ( 'NONE',  ( 2.681043805932831425, 7.005876582393428365, -4.223450101800680478 ) ) ;
#3065 = CARTESIAN_POINT ( 'NONE',  ( -1.492255338562904265, -47.20000000000001705, 11.39999999999999680 ) ) ;
#3066 = ORIENTED_EDGE ( 'NONE', *, *, #2087, .T. ) ;
#3067 = AXIS2_PLACEMENT_3D ( 'NONE', #79, #3091, #1588 ) ;
#3068 = CARTESIAN_POINT ( 'NONE',  ( 3.950486495955891025E-15, -119.2999999999982776, 0.7850000000000663114 ) ) ;
#3069 = FACE_OUTER_BOUND ( 'NONE', #2494, .T. ) ;
#3070 = VERTEX_POINT ( 'NONE', #2148 ) ;
#3071 = CARTESIAN_POINT ( 'NONE',  ( -8.485280282859317680, -50.00000000000000000, 1.400000000000003020 ) ) ;
#3072 = CARTESIAN_POINT ( 'NONE',  ( 8.599999999999996092, -52.79999999999999716, -1.366666666666861873 ) ) ;
#3073 = ORIENTED_EDGE ( 'NONE', *, *, #1816, .T. ) ;
#3074 = CARTESIAN_POINT ( 'NONE',  ( -0.3000000000000161982, -116.3333797136428132, -0.8840511146466779602 ) ) ;
#3075 = CARTESIAN_POINT ( 'NONE',  ( 0.000000000000000000, 0.000000000000000000, 0.000000000000000000 ) ) ;
#3076 = CARTESIAN_POINT ( 'NONE',  ( 0.000000000000000000, -80.00000000000000000, 0.000000000000000000 ) ) ;
#3077 = CARTESIAN_POINT ( 'NONE',  ( 2.500000000000004441, -70.00000000000000000, 0.000000000000000000 ) ) ;
#3078 = ORIENTED_EDGE ( 'NONE', *, *, #889, .F. ) ;
#3079 = CARTESIAN_POINT ( 'NONE',  ( -0.3000000000000037081, -114.9199973783503452, -0.9581324781755546915 ) ) ;
#3080 = PRODUCT_CONTEXT ( 'NONE', #1864, 'mechanical' ) ;
#3081 = CARTESIAN_POINT ( 'NONE',  ( 9.959683570760009985, -47.20000000000001705, 5.743837162466679302 ) ) ;
#3082 = ORIENTED_EDGE ( 'NONE', *, *, #482, .F. ) ;
#3083 = CARTESIAN_POINT ( 'NONE',  ( -4.856127559802944305, -50.91563602443373071, -1.192133730937313008 ) ) ;
#3084 = CARTESIAN_POINT ( 'NONE',  ( 0.000000000000000000, -67.40000000000000568, 2.300000000000000266 ) ) ;
#3085 = VERTEX_POINT ( 'NONE', #1894 ) ;
#3086 = DIRECTION ( 'NONE',  ( 1.000000000000000000, 0.000000000000000000, 0.000000000000000000 ) ) ;
#3087 = EDGE_CURVE ( 'NONE', #356, #2083, #2633, .T. ) ;
#3088 = CARTESIAN_POINT ( 'NONE',  ( 0.000000000000000000, -67.40000000000000568, 0.000000000000000000 ) ) ;
#3089 = CARTESIAN_POINT ( 'NONE',  ( -8.582665138674013150, -52.79999999999999716, 0.5636706063486748297 ) ) ;
#3090 = ORIENTED_EDGE ( 'NONE', *, *, #968, .F. ) ;
#3091 = DIRECTION ( 'NONE',  ( -0.000000000000000000, -0.000000000000000000, 1.000000000000000000 ) ) ;
#3092 = SURFACE_STYLE_USAGE ( .BOTH. , #1606 ) ;
#3093 = EDGE_CURVE ( 'NONE', #2199, #694, #742, .T. ) ;
#3094 = CARTESIAN_POINT ( 'NONE',  ( -2.499999999999994227, -68.53553390593273775, -1.464466094067259805 ) ) ;
#3095 = CARTESIAN_POINT ( 'NONE',  ( -3.359434976081794311, -65.02137218232900295, 3.716172273690825811 ) ) ;
#3096 = CARTESIAN_POINT ( 'NONE',  ( 6.877134118866902845, -50.00000000000000000, 5.285102517562147995 ) ) ;
#3097 = EDGE_LOOP ( 'NONE', ( #2774, #2561, #1329, #1235 ) ) ;
#3098 = DIRECTION ( 'NONE',  ( 0.000000000000000000, 1.000000000000000000, 0.000000000000000000 ) ) ;
#3099 = VECTOR ( 'NONE', #76, 1000.000000000000000 ) ;
#3100 = ADVANCED_FACE ( 'NONE', ( #109 ), #1133, .T. ) ;
#3101 = CARTESIAN_POINT ( 'NONE',  ( -11.39999999999999680, -47.20000000000001705, -1.366666666666159546 ) ) ;
#3102 = AXIS2_PLACEMENT_3D ( 'NONE', #2881, #1854, #656 ) ;
#3103 = ORIENTED_EDGE ( 'NONE', *, *, #2272, .F. ) ;
#3104 = LINE ( 'NONE', #887, #2172 ) ;
#3105 = CARTESIAN_POINT ( 'NONE',  ( 0.2999999999999999889, -114.9199973783503452, 0.9581324781755565789 ) ) ;
#3106 = ORIENTED_EDGE ( 'NONE', *, *, #1477, .T. ) ;
#3107 = CIRCLE ( 'NONE', #248, 2.500000000000000000 ) ;
#3108 = FACE_OUTER_BOUND ( 'NONE', #1963, .T. ) ;
#3109 = CARTESIAN_POINT ( 'NONE',  ( -8.160064090060583197, -52.79999999999999716, 2.773119917861301520 ) ) ;
#3110 = ORIENTED_EDGE ( 'NONE', *, *, #306, .T. ) ;
#3111 = DIRECTION ( 'NONE',  ( -0.000000000000000000, -0.000000000000000000, 1.000000000000000000 ) ) ;
#3112 = SURFACE_STYLE_USAGE ( .BOTH. , #2807 ) ;
#3113 = CARTESIAN_POINT ( 'NONE',  ( 3.767802750538409295, 6.489812437959999514, 3.302060000734929446 ) ) ;
#3114 = LINE ( 'NONE', #1110, #154 ) ;
#3115 = DIRECTION ( 'NONE',  ( 1.000000000000000000, 0.000000000000000000, 0.000000000000000000 ) ) ;
#3116 = ORIENTED_EDGE ( 'NONE', *, *, #1118, .T. ) ;
#3117 = CARTESIAN_POINT ( 'NONE',  ( -4.669423702320314895, 5.869651582198522455, -1.795146503317839759 ) ) ;
#3118 = EDGE_CURVE ( 'NONE', #3153, #1583, #1484, .T. ) ;
#3119 = CIRCLE ( 'NONE', #583, 7.500000000000000000 ) ;
#3120 = CARTESIAN_POINT ( 'NONE',  ( -11.03470001049207916, -50.00000000000000000, 2.958453039083848601 ) ) ;
#3121 = CIRCLE ( 'NONE', #1375, 4.999999999999998224 ) ;
#3122 = EDGE_CURVE ( 'NONE', #2109, #2919, #53, .T. ) ;
#3123 = CARTESIAN_POINT ( 'NONE',  ( -4.954123618475601454, -73.38492426856267059, 0.6974948150963233839 ) ) ;
#3124 = CARTESIAN_POINT ( 'NONE',  ( 1.125736483476999839, -50.00000000000000000, 8.599999999999996092 ) ) ;
#3125 = EDGE_LOOP ( 'NONE', ( #1649, #1071 ) ) ;
#3126 = B_SPLINE_CURVE_WITH_KNOTS ( 'NONE', 3,
 ( #530, #1237, #481, #2559, #1554, #777, #292, #2285, #1491, #12, #274, #1282, #3008, #2048 ),
 .UNSPECIFIED., .F., .F.,
 ( 4, 2, 2, 2, 2, 2, 4 ),
 ( -7.483321517480581097E-06, 0.0003315069634265197353, 0.0006704972483705200475, 0.001348477818258529129, 0.002026458388146537993, 0.002365448673090551641, 0.002704438958034565722 ),
 .UNSPECIFIED. ) ;
#3127 = CARTESIAN_POINT ( 'NONE',  ( -2.417437249938109378, -69.34173728629029654, -4.376918282631313772 ) ) ;
#3128 = DIRECTION ( 'NONE',  ( -0.000000000000000000, -0.000000000000000000, 1.000000000000000000 ) ) ;
#3129 = FACE_BOUND ( 'NONE', #1627, .T. ) ;
#3130 = VERTEX_POINT ( 'NONE', #71 ) ;
#3131 = LINE ( 'NONE', #130, #2698 ) ;
#3132 = CARTESIAN_POINT ( 'NONE',  ( 4.324727228821070746, 6.131211258369285488, 2.529220782163199122 ) ) ;
#3133 = CARTESIAN_POINT ( 'NONE',  ( 11.39999999999999680, -47.20000000000001705, -1.093333333333372126 ) ) ;
#3134 = PRODUCT_DEFINITION_SHAPE ( 'NONE', 'NONE',  #2536 ) ;
#3135 = CARTESIAN_POINT ( 'NONE',  ( -11.39999999999999680, -50.00000000000000711, -1.206666666667079335 ) ) ;
#3136 = ORIENTED_EDGE ( 'NONE', *, *, #2562, .F. ) ;
#3137 = LINE ( 'NONE', #2865, #675 ) ;
#3138 = EDGE_CURVE ( 'NONE', #1508, #38, #747, .T. ) ;
#3139 = CARTESIAN_POINT ( 'NONE',  ( -11.37702123033528778, -50.00000000000000000, 0.7471912688805022462 ) ) ;
#3140 = CARTESIAN_POINT ( 'NONE',  ( 11.64000000000000057, -50.00000000000000000, 0.000000000000000000 ) ) ;
#3141 = ADVANCED_FACE ( 'NONE', ( #2933 ), #2197, .T. ) ;
#3142 = ORIENTED_EDGE ( 'NONE', *, *, #2906, .F. ) ;
#3143 = CARTESIAN_POINT ( 'NONE',  ( -2.499999999999995559, -70.00000000000000000, 0.000000000000000000 ) ) ;
#3144 = LINE ( 'NONE', #60, #2946 ) ;
#3145 = CARTESIAN_POINT ( 'NONE',  ( 8.572527594031472993E-15, -70.00000000000000000, 10.00000000000000000 ) ) ;
#3146 = VERTEX_POINT ( 'NONE', #201 ) ;
#3147 = CARTESIAN_POINT ( 'NONE',  ( 0.000000000000000000, -60.00000000000000000, 2.300000000000000266 ) ) ;
#3148 =( NAMED_UNIT ( * ) PLANE_ANGLE_UNIT ( ) SI_UNIT ( $, .RADIAN. ) );
#3149 = CARTESIAN_POINT ( 'NONE',  ( -9.116201041288242379, -50.00000000000000000, 7.005833569791151128 ) ) ;
#3150 = CARTESIAN_POINT ( 'NONE',  ( -11.39539595717866405, -50.00000000000000000, 0.3739757293043588504 ) ) ;
#3151 = CARTESIAN_POINT ( 'NONE',  ( -4.821318589555972700, 5.745344196342314191, 1.334996645354991074 ) ) ;
#3152 = CARTESIAN_POINT ( 'NONE',  ( 5.742338339643763945, -50.00000000000000000, 9.960716663318306630 ) ) ;
#3153 = VERTEX_POINT ( 'NONE', #1431 ) ;
#3154 = EDGE_CURVE ( 'NONE', #216, #842, #1908, .T. ) ;
#3155 = CARTESIAN_POINT ( 'NONE',  ( -0.8174327128447540503, -72.36830931055405358, -4.935151173937370572 ) ) ;
#3156 = AXIS2_PLACEMENT_3D ( 'NONE', #3076, #2792, #1273 ) ;
#3157 = ORIENTED_EDGE ( 'NONE', *, *, #2125, .T. ) ;
#3158 = PRESENTATION_STYLE_ASSIGNMENT (( #2856 ) ) ;
#3159 = AXIS2_PLACEMENT_3D ( 'NONE', #2960, #2976, #3006 ) ;
#3160 = CYLINDRICAL_SURFACE ( 'NONE', #683, 2.500000000000000444 ) ;
#3161 = CARTESIAN_POINT ( 'NONE',  ( 1.883786463311296844, -68.34852126928106486, -4.633162530913926602 ) ) ;
#3162 = ORIENTED_EDGE ( 'NONE', *, *, #2562, .T. ) ;
#3163 = AXIS2_PLACEMENT_3D ( 'NONE', #1797, #989, #2005 ) ;
#3164 = LINE ( 'NONE', #894, #2957 ) ;
#3165 =( BOUNDED_CURVE ( )  B_SPLINE_CURVE ( 3, ( #3077, #316, #2073, #1575 ),
 .UNSPECIFIED., .F., .F. ) 
 B_SPLINE_CURVE_WITH_KNOTS ( ( 4, 4 ),
 ( 4.712388980384689674, 6.283185307179586232 ),
 .UNSPECIFIED. ) 
 CURVE ( )  GEOMETRIC_REPRESENTATION_ITEM ( )  RATIONAL_B_SPLINE_CURVE ( ( 1.000000000000000000, 0.8047378541243649375, 0.8047378541243649375, 1.000000000000000000 ) ) 
 REPRESENTATION_ITEM ( '' )  );
#3166 = CARTESIAN_POINT ( 'NONE',  ( 8.596526774713710850, -47.20000000000001705, 0.2821220414049827041 ) ) ;
#3167 = CARTESIAN_POINT ( 'NONE',  ( -11.25335008359228794, -50.00000000000000000, 1.860476840075229621 ) ) ;
#3168 = CARTESIAN_POINT ( 'NONE',  ( -0.3000000000000161982, -118.9999999999982379, 0.7416198487096099523 ) ) ;
#3169 = CARTESIAN_POINT ( 'NONE',  ( -11.39999999999999680, -52.79999999999999716, -1.366666666666159546 ) ) ;
#3170 = VERTEX_POINT ( 'NONE', #2039 ) ;
#3171 = AXIS2_PLACEMENT_3D ( 'NONE', #2683, #1422, #908 ) ;
#3172 = CARTESIAN_POINT ( 'NONE',  ( -9.676554491074602637, -48.63437908886124461, 0.3185635799549239588 ) ) ;
#3173 = AXIS2_PLACEMENT_3D ( 'NONE', #1031, #789, #2801 ) ;
#3174 = ORIENTED_EDGE ( 'NONE', *, *, #2147, .T. ) ;
#3175 = CIRCLE ( 'NONE', #318, 7.500000000000000000 ) ;
#3176 = CARTESIAN_POINT ( 'NONE',  ( -1.529827772139811248, -68.01609250619648606, -4.762272014233547068 ) ) ;
#3177 = EDGE_CURVE ( 'NONE', #810, #356, #2778, .T. ) ;
#3178 = CARTESIAN_POINT ( 'NONE',  ( -8.489369361306263073, -50.00000000000000000, 1.403517616197273554 ) ) ;
#3179 = CARTESIAN_POINT ( 'NONE',  ( 0.000000000000000000, 0.000000000000000000, 18.00000000000000355 ) ) ;
#3180 = AXIS2_PLACEMENT_3D ( 'NONE', #1929, #2693, #1966 ) ;
#3181 = EDGE_LOOP ( 'NONE', ( #2346, #2652, #2163, #1659 ) ) ;
#3182 = CARTESIAN_POINT ( 'NONE',  ( 0.000000000000000000, 7.500000000000000000, 4.999999999999999112 ) ) ;
#3183 = CARTESIAN_POINT ( 'NONE',  ( -11.39999999999999680, -47.20000000000001705, -1.639999999999997460 ) ) ;
#3184 = CARTESIAN_POINT ( 'NONE',  ( 0.000000000000000000, 7.500000000000000000, 4.999999999999999112 ) ) ;
#3185 = CARTESIAN_POINT ( 'NONE',  ( 11.37702123033542279, -50.00000000000000000, 0.7471912688806704450 ) ) ;
#3186 = ORIENTED_EDGE ( 'NONE', *, *, #1189, .T. ) ;
#3187 = DIRECTION ( 'NONE',  ( 6.115594274737998660E-18, 0.9987523388778448696, -0.04993761694388874905 ) ) ;
#3188 = DIRECTION ( 'NONE',  ( -0.000000000000000000, -0.000000000000000000, 1.000000000000000000 ) ) ;
#3189 = EDGE_LOOP ( 'NONE', ( #865, #1803, #2292, #1180 ) ) ;
#3190 = CARTESIAN_POINT ( 'NONE',  ( 0.000000000000000000, -125.0000000000000000, 0.000000000000000000 ) ) ;
#3191 = DIRECTION ( 'NONE',  ( 1.000000000000000000, 0.000000000000000000, 0.000000000000000000 ) ) ;
#3192 = DIRECTION ( 'NONE',  ( 1.000000000000000000, 0.000000000000000000, 0.000000000000000000 ) ) ;
#3193 = CARTESIAN_POINT ( 'NONE',  ( 11.39999999999999503, -50.11112248448768014, -1.399999999999995470 ) ) ;
#3194 = EDGE_CURVE ( 'NONE', #84, #2109, #1198, .T. ) ;
#3195 = CARTESIAN_POINT ( 'NONE',  ( 0.000000000000000000, -60.00000000000000000, 0.000000000000000000 ) ) ;
#3196 = CARTESIAN_POINT ( 'NONE',  ( -11.36325033731746004, -50.00000000000000000, 0.9334869871344717573 ) ) ;
#3197 = CARTESIAN_POINT ( 'NONE',  ( -11.37702123033528778, -50.00000000000000000, 0.7471912688805022462 ) ) ;
#3198 = CARTESIAN_POINT ( 'NONE',  ( 0.2999999999999837796, -118.9999999999982379, -2.300000000000000266 ) ) ;
#3199 = CARTESIAN_POINT ( 'NONE',  ( -8.324422814933019055, -52.79999999999999716, 2.231815450536601020 ) ) ;
#3200 = ORIENTED_EDGE ( 'NONE', *, *, #3241, .T. ) ;
#3201 = CARTESIAN_POINT ( 'NONE',  ( -8.530791689320901483, -50.00000000000000000, 1.124695299888049504 ) ) ;
#3202 = DIRECTION ( 'NONE',  ( -1.000000000000000000, 0.000000000000000000, 0.000000000000000000 ) ) ;
#3203 = CARTESIAN_POINT ( 'NONE',  ( 8.572527594031472993E-15, -70.00000000000000000, 0.000000000000000000 ) ) ;
#3204 = EDGE_LOOP ( 'NONE', ( #573, #1020, #917, #802, #2730 ) ) ;
#3205 = CARTESIAN_POINT ( 'NONE',  ( 0.6937423435388915260, -64.03770361543227807, 4.954702760404293471 ) ) ;
#3206 = PRESENTATION_LAYER_ASSIGNMENT (  '', '', ( #982 ) ) ;
#3207 = FACE_OUTER_BOUND ( 'NONE', #933, .T. ) ;
#3208 = DIRECTION ( 'NONE',  ( 0.000000000000000000, -1.000000000000000000, 0.000000000000000000 ) ) ;
#3209 = FACE_OUTER_BOUND ( 'NONE', #352, .T. ) ;
#3210 = CARTESIAN_POINT ( 'NONE',  ( -11.30825875095987421, -52.79999999999999716, 1.490875164968288757 ) ) ;
#3211 = CARTESIAN_POINT ( 'NONE',  ( 4.987611521976591078, -48.54004855990732636, -0.3958319429405975920 ) ) ;
#3212 = CARTESIAN_POINT ( 'NONE',  ( -11.20659079646780221, -50.71729705017419576, -1.206590796467802207 ) ) ;
#3213 = CARTESIAN_POINT ( 'NONE',  ( -8.489369361306263073, -52.79999999999999716, 1.403517616197273554 ) ) ;
#3214 = VERTEX_POINT ( 'NONE', #1022 ) ;
#3215 = CARTESIAN_POINT ( 'NONE',  ( 8.600005876649037262, -50.00000000000000000, -0.2541998246239300374 ) ) ;
#3216 =( NAMED_UNIT ( * ) SI_UNIT ( $, .STERADIAN. ) SOLID_ANGLE_UNIT ( ) );
#3217 = DIRECTION ( 'NONE',  ( -0.000000000000000000, 0.000000000000000000, -1.000000000000000000 ) ) ;
#3218 = ADVANCED_BREP_SHAPE_REPRESENTATION ( '', ( #2670, #1692 ), #1164 ) ;
#3219 = VERTEX_POINT ( 'NONE', #1271 ) ;
#3220 = APPLICATION_CONTEXT ( 'automotive_design' ) ;
#3221 = CARTESIAN_POINT ( 'NONE',  ( 4.325729160396028838, -65.83532677990702098, 2.526449232236036124 ) ) ;
#3222 = VECTOR ( 'NONE', #936, 1000.000000000000000 ) ;
#3223 = AXIS2_PLACEMENT_3D ( 'NONE', #63, #584, #1374 ) ;
#3224 = PLANE ( 'NONE',  #1996 ) ;
#3225 = PRODUCT_RELATED_PRODUCT_CATEGORY ( 'part', '', ( #2159 ) ) ;
#3226 = CARTESIAN_POINT ( 'NONE',  ( 0.000000000000000000, 0.000000000000000000, 18.00000000000000355 ) ) ;
#3227 = CARTESIAN_POINT ( 'NONE',  ( 10.15747651431146892, -51.40000000000001279, -0.1574726270229690750 ) ) ;
#3228 = CIRCLE ( 'NONE', #2014, 7.500000000000000888 ) ;
#3229 = CARTESIAN_POINT ( 'NONE',  ( -4.793596727855903517, -49.51355628789269758, -1.422310562379361487 ) ) ;
#3230 = MECHANICAL_DESIGN_GEOMETRIC_PRESENTATION_REPRESENTATION (  '', ( #2437 ), #2278 ) ;
#3231 = CARTESIAN_POINT ( 'NONE',  ( 11.25335008359272493, -50.00000000000000000, 1.860476840074170246 ) ) ;
#3232 = DIRECTION ( 'NONE',  ( 0.000000000000000000, 0.000000000000000000, 1.000000000000000000 ) ) ;
#3233 = CARTESIAN_POINT ( 'NONE',  ( -9.677496024926982798, -51.36581032562460791, 0.3176491571783061074 ) ) ;
#3234 = CARTESIAN_POINT ( 'NONE',  ( 11.25335008359286704, -52.79999999999999716, 1.860476840074311911 ) ) ;
#3235 = ORIENTED_EDGE ( 'NONE', *, *, #1147, .T. ) ;
#3236 = CARTESIAN_POINT ( 'NONE',  ( -8.572276570256935457, -47.20000000000001705, 0.7042094815226510596 ) ) ;
#3237 = CARTESIAN_POINT ( 'NONE',  ( 1.528985616901159528, -71.98458939899235531, -4.762554006381201965 ) ) ;
#3238 = CARTESIAN_POINT ( 'NONE',  ( 4.327080376399232264, -6.129587957101251483, -2.525419289280399049 ) ) ;
#3239 = CARTESIAN_POINT ( 'NONE',  ( -7.500000000000000000, 0.000000000000000000, 18.00000000000000355 ) ) ;
#3240 = EDGE_CURVE ( 'NONE', #1508, #229, #3037, .T. ) ;
#3241 = EDGE_CURVE ( 'NONE', #2195, #870, #2493, .T. ) ;
#3242 = DIRECTION ( 'NONE',  ( 0.000000000000000000, -1.000000000000000000, 0.000000000000000000 ) ) ;
#3243 = DIRECTION ( 'NONE',  ( 0.000000000000000000, 0.000000000000000000, 1.000000000000000000 ) ) ;
#3244 = ORIENTED_EDGE ( 'NONE', *, *, #230, .T. ) ;
#3245 = CARTESIAN_POINT ( 'NONE',  ( -2.499999999999991118, -70.00000000000000000, 10.00000000000000000 ) ) ;
#3246 = CARTESIAN_POINT ( 'NONE',  ( 11.37702123033549384, -52.79999999999999716, 0.7471912688806703340 ) ) ;
#3247 = DIRECTION ( 'NONE',  ( 0.000000000000000000, -1.000000000000000000, 0.000000000000000000 ) ) ;
#3248 = CARTESIAN_POINT ( 'NONE',  ( -8.906419880262294697, -50.95872650893633704, 1.034857390323304926 ) ) ;
#3249 = CARTESIAN_POINT ( 'NONE',  ( -8.599999999999996092, -50.00000000000000000, -1.639999999999997460 ) ) ;
#3250 = EDGE_LOOP ( 'NONE', ( #2661, #538 ) ) ;
#3251 = CARTESIAN_POINT ( 'NONE',  ( 1.125736483477000061, -47.20000000000001705, 8.599999999999996092 ) ) ;
#3252 = CARTESIAN_POINT ( 'NONE',  ( 1.336826802926396995, -7.387368010283515751, -4.829679162932221992 ) ) ;
#3253 = EDGE_CURVE ( 'NONE', #3000, #2574, #1265, .T. ) ;
#3254 = CARTESIAN_POINT ( 'NONE',  ( 0.000000000000000000, -60.00000000000000000, 0.000000000000000000 ) ) ;
#3255 = CARTESIAN_POINT ( 'NONE',  ( -1.125736483477000061, -47.20000000000001705, 8.599999999999996092 ) ) ;
#3256 = PLANE ( 'NONE',  #1212 ) ;
#3257 = CARTESIAN_POINT ( 'NONE',  ( 11.03475136337292639, -50.94770623811574950, -1.034751363372934829 ) ) ;
#3258 = ADVANCED_FACE ( 'NONE', ( #2478 ), #1726, .T. ) ;
#3259 = AXIS2_PLACEMENT_3D ( 'NONE', #1208, #3232, #1051 ) ;
#3260 = CARTESIAN_POINT ( 'NONE',  ( 0.000000000000000000, 80.00000000000000000, 0.000000000000000000 ) ) ;
#3261 = CARTESIAN_POINT ( 'NONE',  ( -9.116201041287103735, -52.79999999999999716, 7.005833569791151128 ) ) ;
#3262 = CARTESIAN_POINT ( 'NONE',  ( 1.492255338562904043, -50.00000000000000000, 11.39999999999999680 ) ) ;
#3263 = CIRCLE ( 'NONE', #1671, 2.300000000000000266 ) ;
#3264 = CARTESIAN_POINT ( 'NONE',  ( 0.000000000000000000, -67.50000000000000000, -2.500000000000000444 ) ) ;
#3265 = CARTESIAN_POINT ( 'NONE',  ( -8.600005876649037262, -52.79999999999999716, -0.2541998246238979520 ) ) ;
#3266 = VERTEX_POINT ( 'NONE', #170 ) ;
#3267 = AXIS2_PLACEMENT_3D ( 'NONE', #2138, #1881, #633 ) ;
#3268 = LINE ( 'NONE', #997, #1248 ) ;
#3269 = CONTEXT_DEPENDENT_SHAPE_REPRESENTATION ( #1128, #120 ) ;
#3270 = CARTESIAN_POINT ( 'NONE',  ( 0.000000000000000000, -80.00000000000000000, 0.000000000000000000 ) ) ;
#3271 = SHAPE_REPRESENTATION ( 'Needle', ( #1692 ), #1537 ) ;
#3272 = CARTESIAN_POINT ( 'NONE',  ( -4.769696007084728073, -50.09826200962048404, 1.499999999999994449 ) ) ;
#3273 = FACE_OUTER_BOUND ( 'NONE', #2460, .T. ) ;
#3274 = DIRECTION ( 'NONE',  ( 0.000000000000000000, 0.000000000000000000, 1.000000000000000000 ) ) ;
#3275 = CARTESIAN_POINT ( 'NONE',  ( 4.828212536628694984, -49.24633745521808947, 1.300578314244078992 ) ) ;
#3276 = NEXT_ASSEMBLY_USAGE_OCCURRENCE ( 'NAUO1', ' ', ' ', #1297, #1648, $ ) ;
#3277 = NEXT_ASSEMBLY_USAGE_OCCURRENCE ( 'NAUO2', ' ', ' ', #1297, #776, $ ) ;
#3278 = NEXT_ASSEMBLY_USAGE_OCCURRENCE ( 'NAUO3', ' ', ' ', #1297, #2536, $ ) ;
#3279 = NEXT_ASSEMBLY_USAGE_OCCURRENCE ( 'NAUO4', ' ', ' ', #1297, #3057, $ ) ;
#3280=COLOUR_RGB('Dark Blue',0.08,0.2,0.34);
#3281=FILL_AREA_STYLE_COLOUR('',#3280);
#3282=FILL_AREA_STYLE('',(#3281));
#3283=SURFACE_STYLE_FILL_AREA(#3282);
#3284=SURFACE_SIDE_STYLE('',(#3283));
#3285=SURFACE_STYLE_USAGE(.BOTH.,#3284);
#3286=PRESENTATION_STYLE_ASSIGNMENT((#3285));
#3287=COLOUR_RGB('Light Blue',0.38,0.62,0.78);
#3288=FILL_AREA_STYLE_COLOUR('',#3287);
#3289=FILL_AREA_STYLE('',(#3288));
#3290=SURFACE_STYLE_FILL_AREA(#3289);
#3291=SURFACE_SIDE_STYLE('',(#3290));
#3292=SURFACE_STYLE_USAGE(.BOTH.,#3291);
#3293=PRESENTATION_STYLE_ASSIGNMENT((#3292));
#3294=COLOUR_RGB('Sky Blue',0.24,0.69,0.87);
#3295=FILL_AREA_STYLE_COLOUR('',#3294);
#3296=FILL_AREA_STYLE('',(#3295));
#3297=SURFACE_STYLE_FILL_AREA(#3296);
#3298=SURFACE_SIDE_STYLE('',(#3297));
#3299=SURFACE_STYLE_USAGE(.BOTH.,#3298);
#3300=PRESENTATION_STYLE_ASSIGNMENT((#3299));
#3301=COLOUR_RGB('Grey',0.48,0.52,0.57);
#3302=FILL_AREA_STYLE_COLOUR('',#3301);
#3303=FILL_AREA_STYLE('',(#3302));
#3304=SURFACE_STYLE_FILL_AREA(#3303);
#3305=SURFACE_SIDE_STYLE('',(#3304));
#3306=SURFACE_STYLE_USAGE(.BOTH.,#3305);
#3307=PRESENTATION_STYLE_ASSIGNMENT((#3306));
#3308=COLOUR_RGB('Black',0.12,0.14,0.17);
#3309=FILL_AREA_STYLE_COLOUR('',#3308);
#3310=FILL_AREA_STYLE('',(#3309));
#3311=SURFACE_STYLE_FILL_AREA(#3310);
#3312=SURFACE_SIDE_STYLE('',(#3311));
#3313=SURFACE_STYLE_USAGE(.BOTH.,#3312);
#3314=PRESENTATION_STYLE_ASSIGNMENT((#3313));
#3315=COLOUR_RGB('Off White',0.89,0.88,0.83);
#3316=FILL_AREA_STYLE_COLOUR('',#3315);
#3317=FILL_AREA_STYLE('',(#3316));
#3318=SURFACE_STYLE_FILL_AREA(#3317);
#3319=SURFACE_SIDE_STYLE('',(#3318));
#3320=SURFACE_STYLE_USAGE(.BOTH.,#3319);
#3321=PRESENTATION_STYLE_ASSIGNMENT((#3320));
ENDSEC;
END-ISO-10303-21;
